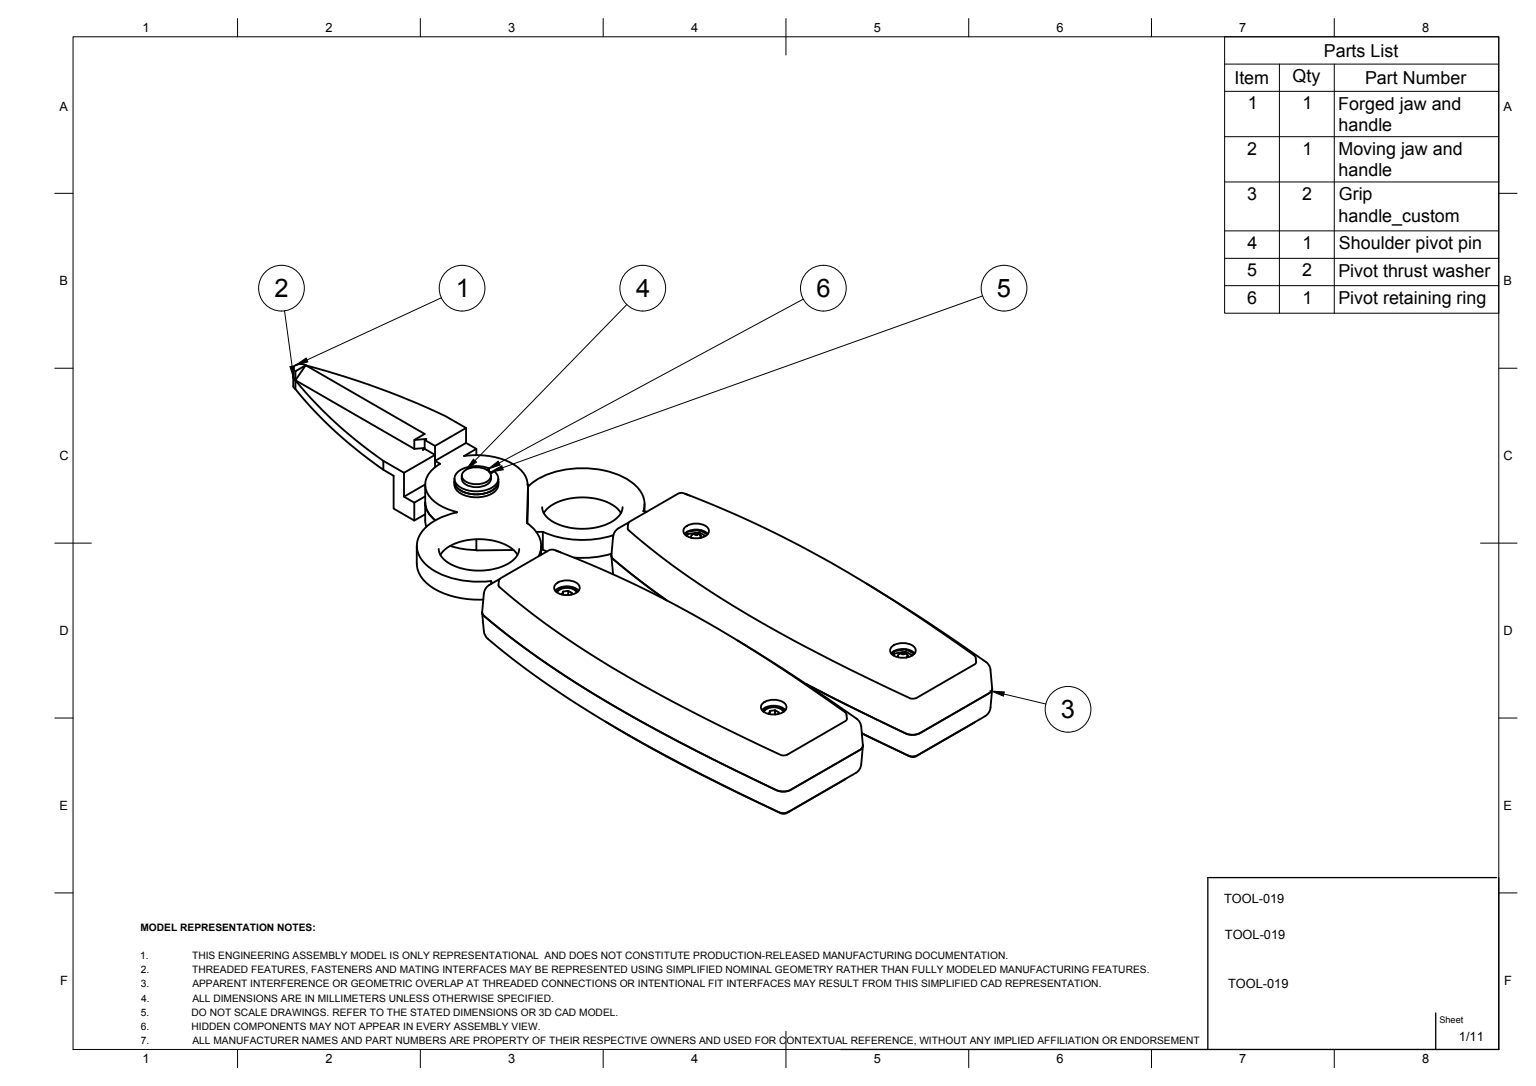
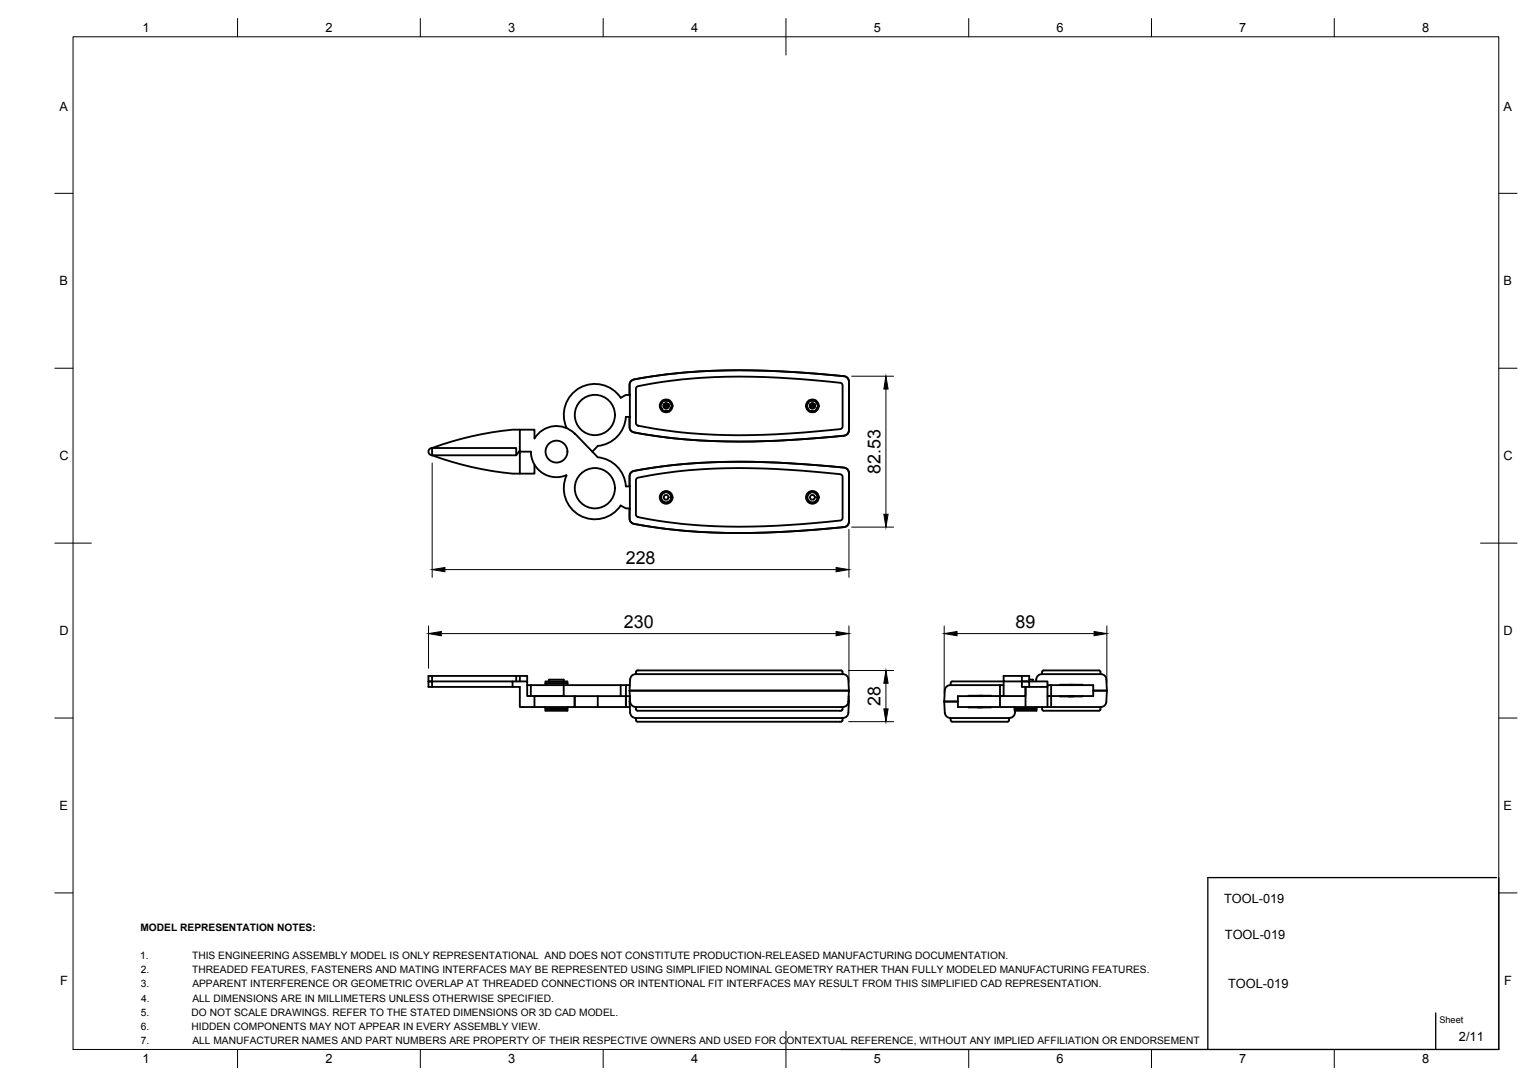
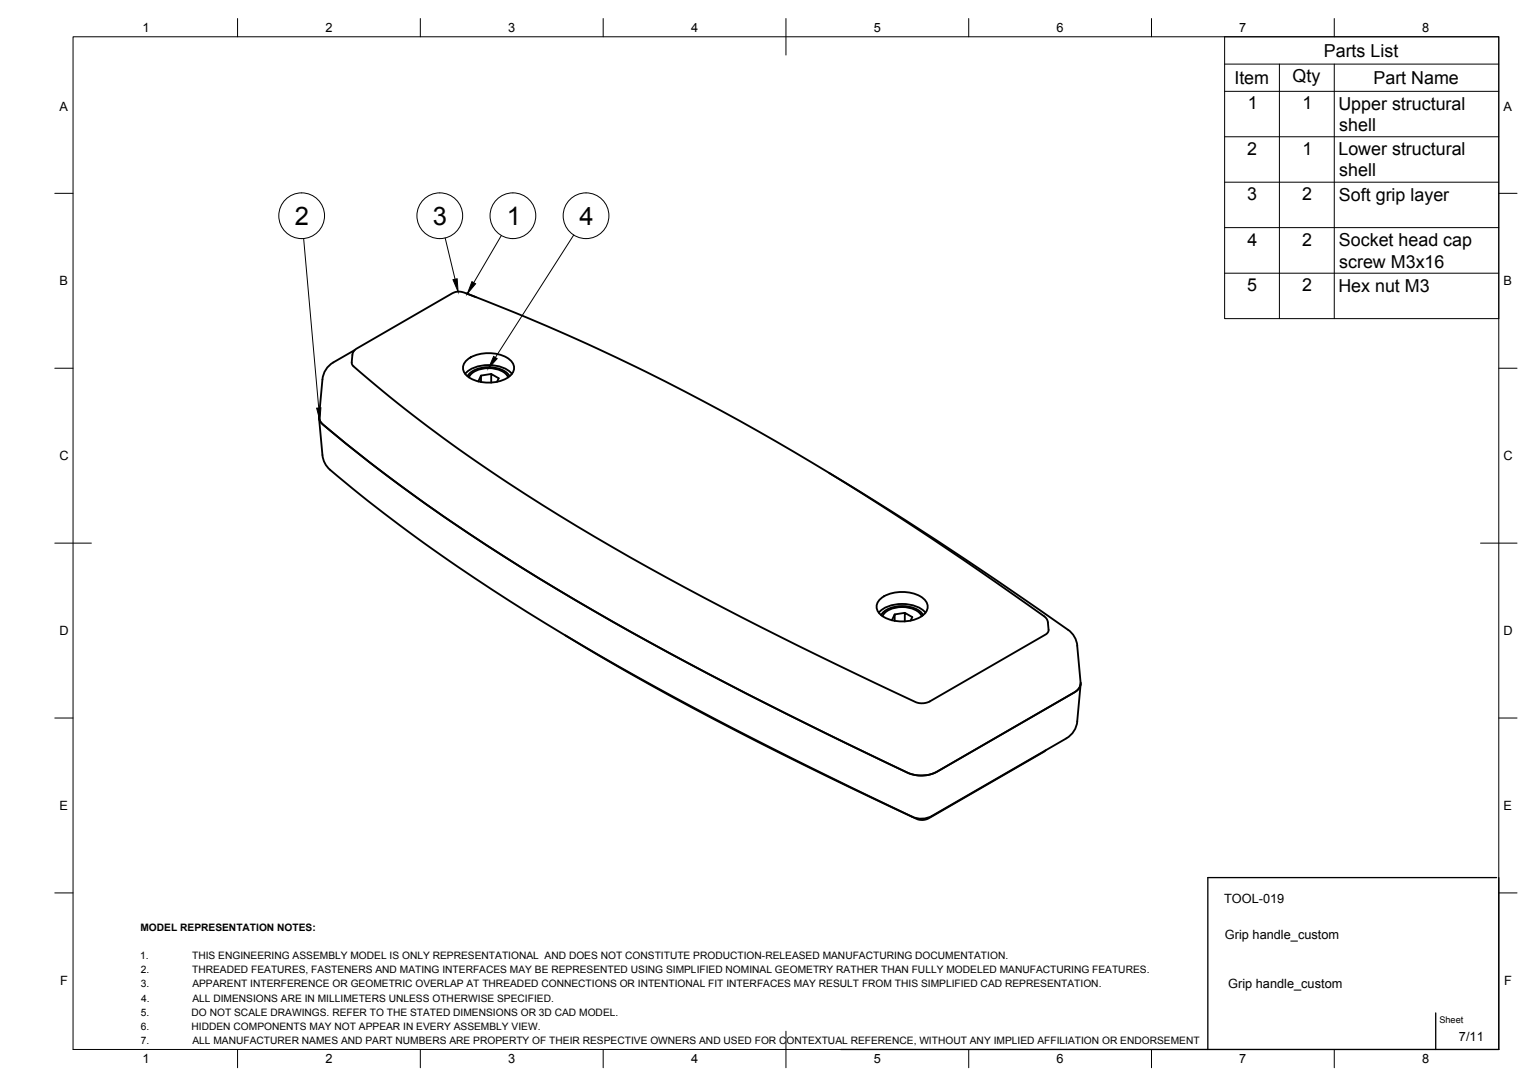
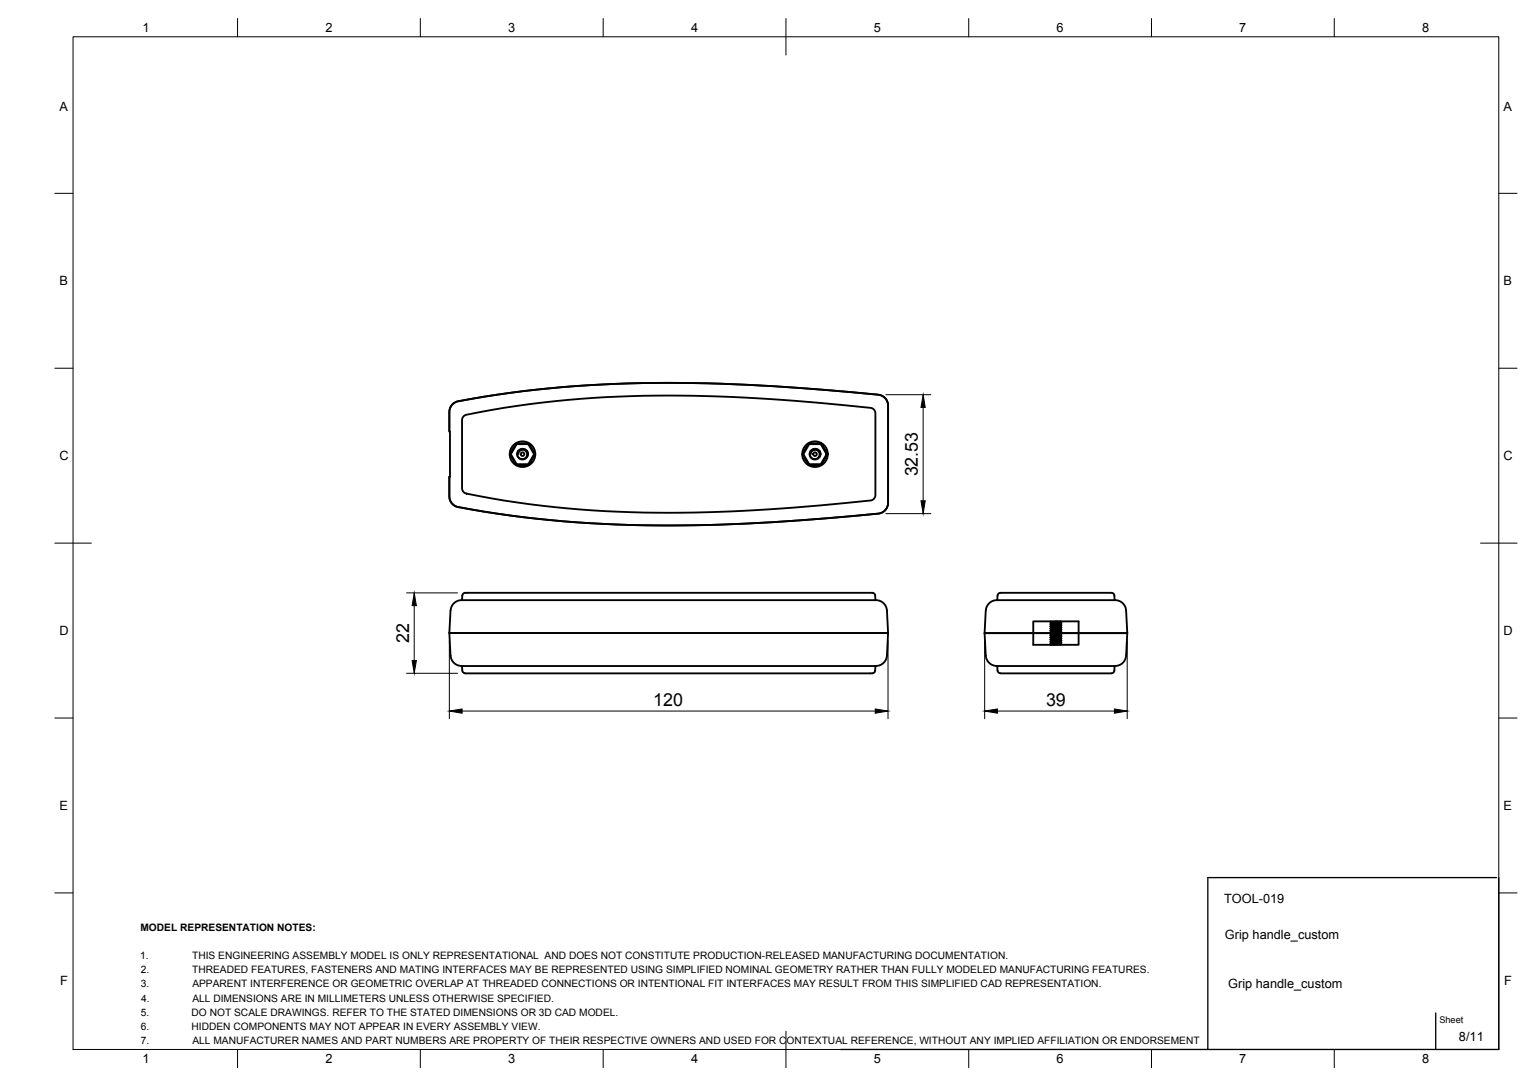
ISO-10303-21;
HEADER;
/* Generated by software containing ST-Developer
 * from STEP Tools, Inc. (www.steptools.com) 
 */

FILE_DESCRIPTION(
/* description */ (''),
/* implementation_level */ '2;1');

FILE_NAME(
/* name */ 'TOOL-019.step',
/* time_stamp */ '2026-11-10T09:14:46-08:00',
/* author */ (''),
/* organization */ (''),
/* preprocessor_version */ 'ST-DEVELOPER v20.2',
/* originating_system */ 'Autodesk Translation Framework v15.17.0.0',
/* authorisation */ '');

FILE_SCHEMA (('AUTOMOTIVE_DESIGN { 1 0 10303 214 3 1 1 }'));
ENDSEC;

DATA;
#10=MECHANICAL_DESIGN_GEOMETRIC_PRESENTATION_REPRESENTATION('',(#558,#559,
#560,#561,#562,#563,#564,#565,#566,#567),#19471);
#11=ITEM_DEFINED_TRANSFORMATION($,$,#7423,#7794);
#12=ITEM_DEFINED_TRANSFORMATION($,$,#7525,#7795);
#13=ITEM_DEFINED_TRANSFORMATION($,$,#7633,#7796);
#14=ITEM_DEFINED_TRANSFORMATION($,$,#7686,#7797);
#15=ITEM_DEFINED_TRANSFORMATION($,$,#7768,#7798);
#16=ITEM_DEFINED_TRANSFORMATION($,$,#7633,#7799);
#17=ITEM_DEFINED_TRANSFORMATION($,$,#7686,#7800);
#18=ITEM_DEFINED_TRANSFORMATION($,$,#7768,#7801);
#19=ITEM_DEFINED_TRANSFORMATION($,$,#7273,#7811);
#20=ITEM_DEFINED_TRANSFORMATION($,$,#7333,#7812);
#21=ITEM_DEFINED_TRANSFORMATION($,$,#7422,#7813);
#22=ITEM_DEFINED_TRANSFORMATION($,$,#7393,#7814);
#23=ITEM_DEFINED_TRANSFORMATION($,$,#7802,#7815);
#24=ITEM_DEFINED_TRANSFORMATION($,$,#7411,#7816);
#25=ITEM_DEFINED_TRANSFORMATION($,$,#7422,#7817);
#26=ITEM_DEFINED_TRANSFORMATION($,$,#7802,#7818);
#27=(
REPRESENTATION_RELATIONSHIP($,$,#19522,#19521)
REPRESENTATION_RELATIONSHIP_WITH_TRANSFORMATION(#11)
SHAPE_REPRESENTATION_RELATIONSHIP()
);
#28=(
REPRESENTATION_RELATIONSHIP($,$,#19523,#19521)
REPRESENTATION_RELATIONSHIP_WITH_TRANSFORMATION(#12)
SHAPE_REPRESENTATION_RELATIONSHIP()
);
#29=(
REPRESENTATION_RELATIONSHIP($,$,#19524,#19521)
REPRESENTATION_RELATIONSHIP_WITH_TRANSFORMATION(#13)
SHAPE_REPRESENTATION_RELATIONSHIP()
);
#30=(
REPRESENTATION_RELATIONSHIP($,$,#19525,#19521)
REPRESENTATION_RELATIONSHIP_WITH_TRANSFORMATION(#14)
SHAPE_REPRESENTATION_RELATIONSHIP()
);
#31=(
REPRESENTATION_RELATIONSHIP($,$,#19526,#19521)
REPRESENTATION_RELATIONSHIP_WITH_TRANSFORMATION(#15)
SHAPE_REPRESENTATION_RELATIONSHIP()
);
#32=(
REPRESENTATION_RELATIONSHIP($,$,#19524,#19521)
REPRESENTATION_RELATIONSHIP_WITH_TRANSFORMATION(#16)
SHAPE_REPRESENTATION_RELATIONSHIP()
);
#33=(
REPRESENTATION_RELATIONSHIP($,$,#19525,#19521)
REPRESENTATION_RELATIONSHIP_WITH_TRANSFORMATION(#17)
SHAPE_REPRESENTATION_RELATIONSHIP()
);
#34=(
REPRESENTATION_RELATIONSHIP($,$,#19526,#19521)
REPRESENTATION_RELATIONSHIP_WITH_TRANSFORMATION(#18)
SHAPE_REPRESENTATION_RELATIONSHIP()
);
#35=(
REPRESENTATION_RELATIONSHIP($,$,#19517,#19516)
REPRESENTATION_RELATIONSHIP_WITH_TRANSFORMATION(#19)
SHAPE_REPRESENTATION_RELATIONSHIP()
);
#36=(
REPRESENTATION_RELATIONSHIP($,$,#19518,#19516)
REPRESENTATION_RELATIONSHIP_WITH_TRANSFORMATION(#20)
SHAPE_REPRESENTATION_RELATIONSHIP()
);
#37=(
REPRESENTATION_RELATIONSHIP($,$,#19521,#19516)
REPRESENTATION_RELATIONSHIP_WITH_TRANSFORMATION(#21)
SHAPE_REPRESENTATION_RELATIONSHIP()
);
#38=(
REPRESENTATION_RELATIONSHIP($,$,#19519,#19516)
REPRESENTATION_RELATIONSHIP_WITH_TRANSFORMATION(#22)
SHAPE_REPRESENTATION_RELATIONSHIP()
);
#39=(
REPRESENTATION_RELATIONSHIP($,$,#19527,#19516)
REPRESENTATION_RELATIONSHIP_WITH_TRANSFORMATION(#23)
SHAPE_REPRESENTATION_RELATIONSHIP()
);
#40=(
REPRESENTATION_RELATIONSHIP($,$,#19520,#19516)
REPRESENTATION_RELATIONSHIP_WITH_TRANSFORMATION(#24)
SHAPE_REPRESENTATION_RELATIONSHIP()
);
#41=(
REPRESENTATION_RELATIONSHIP($,$,#19521,#19516)
REPRESENTATION_RELATIONSHIP_WITH_TRANSFORMATION(#25)
SHAPE_REPRESENTATION_RELATIONSHIP()
);
#42=(
REPRESENTATION_RELATIONSHIP($,$,#19527,#19516)
REPRESENTATION_RELATIONSHIP_WITH_TRANSFORMATION(#26)
SHAPE_REPRESENTATION_RELATIONSHIP()
);
#43=CONTEXT_DEPENDENT_SHAPE_REPRESENTATION(#27,#19499);
#44=CONTEXT_DEPENDENT_SHAPE_REPRESENTATION(#28,#19500);
#45=CONTEXT_DEPENDENT_SHAPE_REPRESENTATION(#29,#19501);
#46=CONTEXT_DEPENDENT_SHAPE_REPRESENTATION(#30,#19502);
#47=CONTEXT_DEPENDENT_SHAPE_REPRESENTATION(#31,#19503);
#48=CONTEXT_DEPENDENT_SHAPE_REPRESENTATION(#32,#19504);
#49=CONTEXT_DEPENDENT_SHAPE_REPRESENTATION(#33,#19505);
#50=CONTEXT_DEPENDENT_SHAPE_REPRESENTATION(#34,#19506);
#51=CONTEXT_DEPENDENT_SHAPE_REPRESENTATION(#35,#19508);
#52=CONTEXT_DEPENDENT_SHAPE_REPRESENTATION(#36,#19509);
#53=CONTEXT_DEPENDENT_SHAPE_REPRESENTATION(#37,#19510);
#54=CONTEXT_DEPENDENT_SHAPE_REPRESENTATION(#38,#19511);
#55=CONTEXT_DEPENDENT_SHAPE_REPRESENTATION(#39,#19512);
#56=CONTEXT_DEPENDENT_SHAPE_REPRESENTATION(#40,#19513);
#57=CONTEXT_DEPENDENT_SHAPE_REPRESENTATION(#41,#19514);
#58=CONTEXT_DEPENDENT_SHAPE_REPRESENTATION(#42,#19515);
#59=NEXT_ASSEMBLY_USAGE_OCCURRENCE('Upper structural shell:1',
'Upper structural shell:1','Upper structural shell:1',#19534,#19535,
'Upper structural shell:1');
#60=NEXT_ASSEMBLY_USAGE_OCCURRENCE('Lower structural shell:1',
'Lower structural shell:1','Lower structural shell:1',#19534,#19536,
'Lower structural shell:1');
#61=NEXT_ASSEMBLY_USAGE_OCCURRENCE('Soft grip layer:1',
'Soft grip layer:1','Soft grip layer:1',#19534,#19537,
'Soft grip layer:1');
#62=NEXT_ASSEMBLY_USAGE_OCCURRENCE('Socket head cap screw M3x16:1',
'Socket head cap screw M3x16:1','Socket head cap screw M3x16:1',#19534,
#19538,'Socket head cap screw M3x16:1');
#63=NEXT_ASSEMBLY_USAGE_OCCURRENCE('Hex nut M3:1','Hex nut M3:1',
'Hex nut M3:1',#19534,#19539,'Hex nut M3:1');
#64=NEXT_ASSEMBLY_USAGE_OCCURRENCE('Soft grip layer:2',
'Soft grip layer:2','Soft grip layer:2',#19534,#19537,
'Soft grip layer:2');
#65=NEXT_ASSEMBLY_USAGE_OCCURRENCE('Socket head cap screw M3x16:2',
'Socket head cap screw M3x16:2','Socket head cap screw M3x16:2',#19534,
#19538,'Socket head cap screw M3x16:2');
#66=NEXT_ASSEMBLY_USAGE_OCCURRENCE('Hex nut M3:2','Hex nut M3:2',
'Hex nut M3:2',#19534,#19539,'Hex nut M3:2');
#67=NEXT_ASSEMBLY_USAGE_OCCURRENCE('Forged jaw and handle:1',
'Forged jaw and handle:1','Forged jaw and handle:1',#19529,#19530,
'Forged jaw and handle:1');
#68=NEXT_ASSEMBLY_USAGE_OCCURRENCE('Moving jaw and handle:1',
'Moving jaw and handle:1','Moving jaw and handle:1',#19529,#19531,
'Moving jaw and handle:1');
#69=NEXT_ASSEMBLY_USAGE_OCCURRENCE('Grip handle_custom:1',
'Grip handle_custom:1','Grip handle_custom:1',#19529,#19534,
'Grip handle_custom:1');
#70=NEXT_ASSEMBLY_USAGE_OCCURRENCE('Shoulder pivot pin:1',
'Shoulder pivot pin:1','Shoulder pivot pin:1',#19529,#19532,
'Shoulder pivot pin:1');
#71=NEXT_ASSEMBLY_USAGE_OCCURRENCE('Pivot thrust washer:1',
'Pivot thrust washer:1','Pivot thrust washer:1',#19529,#19540,
'Pivot thrust washer:1');
#72=NEXT_ASSEMBLY_USAGE_OCCURRENCE('Pivot retaining ring:1',
'Pivot retaining ring:1','Pivot retaining ring:1',#19529,#19533,
'Pivot retaining ring:1');
#73=NEXT_ASSEMBLY_USAGE_OCCURRENCE('Grip handle_custom:2',
'Grip handle_custom:2','Grip handle_custom:2',#19529,#19534,
'Grip handle_custom:2');
#74=NEXT_ASSEMBLY_USAGE_OCCURRENCE('Pivot thrust washer:2',
'Pivot thrust washer:2','Pivot thrust washer:2',#19529,#19540,
'Pivot thrust washer:2');
#75=CONICAL_SURFACE('',#7749,0.1,0.785398163397448);
#76=SPHERICAL_SURFACE('',#7488,0.0999999999999999);
#77=SPHERICAL_SURFACE('',#7491,0.100000000000002);
#78=SPHERICAL_SURFACE('',#7495,0.0999999999999991);
#79=SPHERICAL_SURFACE('',#7499,0.1);
#80=SPHERICAL_SURFACE('',#7504,0.3);
#81=SPHERICAL_SURFACE('',#7508,0.300000000000002);
#82=SPHERICAL_SURFACE('',#7512,0.299999999999999);
#83=SPHERICAL_SURFACE('',#7517,0.3);
#84=SPHERICAL_SURFACE('',#7596,0.0999999999999999);
#85=SPHERICAL_SURFACE('',#7599,0.100000000000002);
#86=SPHERICAL_SURFACE('',#7603,0.0999999999999991);
#87=SPHERICAL_SURFACE('',#7607,0.1);
#88=SPHERICAL_SURFACE('',#7612,0.3);
#89=SPHERICAL_SURFACE('',#7616,0.300000000000002);
#90=SPHERICAL_SURFACE('',#7620,0.299999999999999);
#91=SPHERICAL_SURFACE('',#7625,0.3);
#92=B_SPLINE_SURFACE_WITH_KNOTS('',3,3,((#10686,#10687,#10688,#10689),(#10690,
#10691,#10692,#10693),(#10694,#10695,#10696,#10697),(#10698,#10699,#10700,
#10701)),.UNSPECIFIED.,.F.,.F.,.F.,(4,4),(4,4),(0.0627625298587661,0.3242096015809),
(0.0118073085896899,0.685451490706028),.UNSPECIFIED.);
#93=B_SPLINE_SURFACE_WITH_KNOTS('',3,3,((#10706,#10707,#10708,#10709),(#10710,
#10711,#10712,#10713),(#10714,#10715,#10716,#10717),(#10718,#10719,#10720,
#10721)),.UNSPECIFIED.,.F.,.F.,.F.,(4,4),(4,4),(0.0225360950145449,0.0483865590996774),
(0.0125659096559557,0.685650832343257),.UNSPECIFIED.);
#94=B_SPLINE_SURFACE_WITH_KNOTS('',3,3,((#10731,#10732,#10733,#10734),(#10735,
#10736,#10737,#10738),(#10739,#10740,#10741,#10742),(#10743,#10744,#10745,
#10746),(#10747,#10748,#10749,#10750)),.UNSPECIFIED.,.F.,.F.,.F.,(4,1,4),
(4,4),(0.,0.571428571428571,1.),(0.74118252158834,3.85438678954986),
 .UNSPECIFIED.);
#95=B_SPLINE_SURFACE_WITH_KNOTS('',3,3,((#10755,#10756,#10757,#10758),(#10759,
#10760,#10761,#10762),(#10763,#10764,#10765,#10766),(#10767,#10768,#10769,
#10770),(#10771,#10772,#10773,#10774)),.UNSPECIFIED.,.F.,.F.,.F.,(4,1,4),
(4,4),(0.,0.571428571428571,1.),(0.270878787657975,0.54981857912664),
 .UNSPECIFIED.);
#96=B_SPLINE_SURFACE_WITH_KNOTS('',3,3,((#10793,#10794,#10795,#10796),(#10797,
#10798,#10799,#10800),(#10801,#10802,#10803,#10804),(#10805,#10806,#10807,
#10808),(#10809,#10810,#10811,#10812)),.UNSPECIFIED.,.F.,.F.,.F.,(4,1,4),
(4,4),(0.,0.571428571428571,1.),(8.03948512627517,11.1526893942367),
 .UNSPECIFIED.);
#97=B_SPLINE_SURFACE_WITH_KNOTS('',3,3,((#10817,#10818,#10819,#10820),(#10821,
#10822,#10823,#10824),(#10825,#10826,#10827,#10828),(#10829,#10830,#10831,
#10832)),.UNSPECIFIED.,.F.,.F.,.F.,(4,4),(4,4),(0.675790398419059,0.937237470141233),
(0.0118073085603101,0.685451490706029),.UNSPECIFIED.);
#98=B_SPLINE_SURFACE_WITH_KNOTS('',3,3,((#10833,#10834,#10835,#10836),(#10837,
#10838,#10839,#10840),(#10841,#10842,#10843,#10844),(#10845,#10846,#10847,
#10848)),.UNSPECIFIED.,.F.,.F.,.F.,(4,4),(4,4),(0.951613440900322,0.977463904985455),
(0.0125659096559558,0.685650832343257),.UNSPECIFIED.);
#99=B_SPLINE_SURFACE_WITH_KNOTS('',3,3,((#10932,#10933,#10934,#10935),(#10936,
#10937,#10938,#10939),(#10940,#10941,#10942,#10943),(#10944,#10945,#10946,
#10947)),.UNSPECIFIED.,.F.,.F.,.F.,(4,4),(4,4),(0.340089900275858,0.660082688299826),
(0.0116294244283504,0.684384408933581),.UNSPECIFIED.);
#100=B_SPLINE_SURFACE_WITH_KNOTS('',3,3,((#10952,#10953,#10954,#10955),
(#10956,#10957,#10958,#10959),(#10960,#10961,#10962,#10963),(#10964,#10965,
#10966,#10967),(#10968,#10969,#10970,#10971)),.UNSPECIFIED.,.F.,.F.,.F.,
(4,1,4),(4,4),(0.,0.571428571428571,1.),(4.04989375377528,7.85140214144331),
 .UNSPECIFIED.);
#101=B_SPLINE_SURFACE_WITH_KNOTS('',3,3,((#10981,#10982,#10983,#10984),
(#10985,#10986,#10987,#10988),(#10989,#10990,#10991,#10992),(#10993,#10994,
#10995,#10996),(#10997,#10998,#10999,#11000)),.UNSPECIFIED.,.F.,.F.,.F.,
(4,1,4),(4,4),(0.,0.571428571428571,1.),(4.0424697743818,7.84397816204974),
 .UNSPECIFIED.);
#102=B_SPLINE_SURFACE_WITH_KNOTS('',3,3,((#11005,#11006,#11007,#11008),
(#11009,#11010,#11011,#11012),(#11013,#11014,#11015,#11016),(#11017,#11018,
#11019,#11020)),.UNSPECIFIED.,.F.,.F.,.F.,(4,4),(4,4),(0.339917311700174,
0.659910099724142),(0.0116294573698948,0.684384408933581),.UNSPECIFIED.);
#103=B_SPLINE_SURFACE_WITH_KNOTS('',3,3,((#11095,#11096,#11097,#11098),
(#11099,#11100,#11101,#11102),(#11103,#11104,#11105,#11106),(#11107,#11108,
#11109,#11110)),.UNSPECIFIED.,.F.,.F.,.F.,(4,4),(4,4),(0.675996615945502,
0.913173856075534),(0.0118505108223707,0.686152089762332),.UNSPECIFIED.);
#104=B_SPLINE_SURFACE_WITH_KNOTS('',3,3,((#11115,#11116,#11117,#11118),
(#11119,#11120,#11121,#11122),(#11123,#11124,#11125,#11126),(#11127,#11128,
#11129,#11130),(#11131,#11132,#11133,#11134)),.UNSPECIFIED.,.F.,.F.,.F.,
(4,1,4),(4,4),(0.,0.571428571428571,1.),(8.0457708503995,10.8690635835914),
 .UNSPECIFIED.);
#105=B_SPLINE_SURFACE_WITH_KNOTS('',3,3,((#11144,#11145,#11146,#11147),
(#11148,#11149,#11150,#11151),(#11152,#11153,#11154,#11155),(#11156,#11157,
#11158,#11159),(#11160,#11161,#11162,#11163)),.UNSPECIFIED.,.F.,.F.,.F.,
(4,1,4),(4,4),(0.,0.571428571428571,1.),(1.02480833223363,3.8481010654256),
 .UNSPECIFIED.);
#106=B_SPLINE_SURFACE_WITH_KNOTS('',3,3,((#11168,#11169,#11170,#11171),
(#11172,#11173,#11174,#11175),(#11176,#11177,#11178,#11179),(#11180,#11181,
#11182,#11183)),.UNSPECIFIED.,.F.,.F.,.F.,(4,4),(4,4),(0.0868261439244655,
0.324003384054498),(0.0118505108223707,0.686152089762332),.UNSPECIFIED.);
#107=B_SPLINE_SURFACE_WITH_KNOTS('',3,3,((#11258,#11259,#11260,#11261),
(#11262,#11263,#11264,#11265),(#11266,#11267,#11268,#11269),(#11270,#11271,
#11272,#11273)),.UNSPECIFIED.,.F.,.F.,.F.,(4,4),(4,4),(0.927751606342899,
0.979699913047832),(0.0130895688562318,0.686930956013783),.UNSPECIFIED.);
#108=B_SPLINE_SURFACE_WITH_KNOTS('',3,3,((#11283,#11284,#11285,#11286),
(#11287,#11288,#11289,#11290),(#11291,#11292,#11293,#11294),(#11295,#11296,
#11297,#11298),(#11299,#11300,#11301,#11302)),.UNSPECIFIED.,.F.,.F.,.F.,
(4,1,4),(4,4),(0.,0.571428571428571,1.),(11.0550486447215,11.6488871259622),
 .UNSPECIFIED.);
#109=B_SPLINE_SURFACE_WITH_KNOTS('',3,3,((#11316,#11317,#11318,#11319),
(#11320,#11321,#11322,#11323),(#11324,#11325,#11326,#11327),(#11328,#11329,
#11330,#11331)),.UNSPECIFIED.,.F.,.F.,.F.,(4,4),(4,4),(0.0203000869521683,
0.0722483936571013),(0.0130895688562318,0.686930956013783),
 .UNSPECIFIED.);
#110=B_SPLINE_SURFACE_WITH_KNOTS('',3,3,((#11341,#11342,#11343,#11344),
(#11345,#11346,#11347,#11348),(#11349,#11350,#11351,#11352),(#11353,#11354,
#11355,#11356),(#11357,#11358,#11359,#11360)),.UNSPECIFIED.,.F.,.F.,.F.,
(4,1,4),(4,4),(0.,0.571428571428571,1.),(0.244984789862841,0.838823271103535),
 .UNSPECIFIED.);
#111=B_SPLINE_SURFACE_WITH_KNOTS('',3,3,((#11374,#11375,#11376,#11377),
(#11378,#11379,#11380,#11381),(#11382,#11383,#11384,#11385),(#11386,#11387,
#11388,#11389),(#11390,#11391,#11392,#11393)),.UNSPECIFIED.,.F.,.F.,.F.,
(4,1,4),(4,4),(0.,0.5,1.),(0.0108921325678979,0.619909717328002),
 .UNSPECIFIED.);
#112=B_SPLINE_SURFACE_WITH_KNOTS('',3,3,((#11400,#11401,#11402,#11403),
(#11404,#11405,#11406,#11407),(#11408,#11409,#11410,#11411),(#11412,#11413,
#11414,#11415),(#11416,#11417,#11418,#11419)),.UNSPECIFIED.,.F.,.F.,.F.,
(4,1,4),(4,4),(0.,0.571428571428571,1.),(0.00967450486392679,0.618764321025346),
 .UNSPECIFIED.);
#113=B_SPLINE_SURFACE_WITH_KNOTS('',3,3,((#11424,#11425,#11426,#11427),
(#11428,#11429,#11430,#11431),(#11432,#11433,#11434,#11435),(#11436,#11437,
#11438,#11439),(#11440,#11441,#11442,#11443)),.UNSPECIFIED.,.F.,.F.,.F.,
(4,1,4),(4,4),(0.,0.571428571428571,1.),(0.0097274579809394,0.618764321025346),
 .UNSPECIFIED.);
#114=B_SPLINE_SURFACE_WITH_KNOTS('',3,3,((#11448,#11449,#11450,#11451),
(#11452,#11453,#11454,#11455),(#11456,#11457,#11458,#11459),(#11460,#11461,
#11462,#11463),(#11464,#11465,#11466,#11467)),.UNSPECIFIED.,.F.,.F.,.F.,
(4,1,4),(4,4),(0.,0.571428571428571,1.),(11.3440533366984,11.6229931281671),
 .UNSPECIFIED.);
#115=B_SPLINE_SURFACE_WITH_KNOTS('',3,3,((#11468,#11469,#11470,#11471),
(#11472,#11473,#11474,#11475),(#11476,#11477,#11478,#11479),(#11480,#11481,
#11482,#11483),(#11484,#11485,#11486,#11487)),.UNSPECIFIED.,.F.,.F.,.F.,
(4,1,4),(4,4),(0.,0.5,1.),(0.0108402259132964,0.619909717328002),
 .UNSPECIFIED.);
#116=B_SPLINE_SURFACE_WITH_KNOTS('',3,3,((#11513,#11514,#11515,#11516),
(#11517,#11518,#11519,#11520),(#11521,#11522,#11523,#11524),(#11525,#11526,
#11527,#11528),(#11529,#11530,#11531,#11532)),.UNSPECIFIED.,.F.,.F.,.F.,
(4,1,4),(4,4),(0.,0.571428571428571,1.),(-0.00387706229521417,0.619909717328002),
 .UNSPECIFIED.);
#117=B_SPLINE_SURFACE_WITH_KNOTS('',3,3,((#11551,#11552,#11553,#11554,#11555,
#11556),(#11557,#11558,#11559,#11560,#11561,#11562),(#11563,#11564,#11565,
#11566,#11567,#11568),(#11569,#11570,#11571,#11572,#11573,#11574),(#11575,
#11576,#11577,#11578,#11579,#11580)),.UNSPECIFIED.,.F.,.F.,.F.,(4,1,4),
(4,1,1,4),(0.,0.571428571428571,1.),(0.270878787657975,5.14716807550265,
8.39802760073243,11.6488871259622),.UNSPECIFIED.);
#118=B_SPLINE_SURFACE_WITH_KNOTS('',3,3,((#11593,#11594,#11595,#11596),
(#11597,#11598,#11599,#11600),(#11601,#11602,#11603,#11604),(#11605,#11606,
#11607,#11608),(#11609,#11610,#11611,#11612)),.UNSPECIFIED.,.F.,.F.,.F.,
(4,1,4),(4,4),(0.,0.571428571428571,1.),(-0.00522825793187074,0.618764321025346),
 .UNSPECIFIED.);
#119=B_SPLINE_SURFACE_WITH_KNOTS('',3,3,((#11621,#11622,#11623,#11624),
(#11625,#11626,#11627,#11628),(#11629,#11630,#11631,#11632),(#11633,#11634,
#11635,#11636),(#11637,#11638,#11639,#11640)),.UNSPECIFIED.,.F.,.F.,.F.,
(4,1,4),(4,4),(0.,0.571428571428571,1.),(-0.00506942997988007,0.618764321025346),
 .UNSPECIFIED.);
#120=B_SPLINE_SURFACE_WITH_KNOTS('',3,3,((#11649,#11650,#11651,#11652,#11653),
(#11654,#11655,#11656,#11657,#11658),(#11659,#11660,#11661,#11662,#11663),
(#11664,#11665,#11666,#11667,#11668),(#11669,#11670,#11671,#11672,#11673)),
 .UNSPECIFIED.,.F.,.F.,.F.,(4,1,4),(4,1,4),(0.,0.571428571428571,1.),(0.244984789862841,
5.12127407770751,11.6229931281671),.UNSPECIFIED.);
#121=B_SPLINE_SURFACE_WITH_KNOTS('',3,3,((#11684,#11685,#11686,#11687),
(#11688,#11689,#11690,#11691),(#11692,#11693,#11694,#11695),(#11696,#11697,
#11698,#11699),(#11700,#11701,#11702,#11703)),.UNSPECIFIED.,.F.,.F.,.F.,
(4,1,4),(4,4),(0.,0.571428571428571,1.),(-0.00403278922781227,0.619909717328002),
 .UNSPECIFIED.);
#122=B_SPLINE_SURFACE_WITH_KNOTS('',3,3,((#11712,#11713,#11714,#11715),
(#11716,#11717,#11718,#11719),(#11720,#11721,#11722,#11723),(#11724,#11725,
#11726,#11727)),.UNSPECIFIED.,.F.,.F.,.F.,(4,4),(4,4),(0.0225340877622934,
0.979701609653785),(0.,0.686930956013783),.UNSPECIFIED.);
#123=B_SPLINE_SURFACE_WITH_KNOTS('',3,3,((#11730,#11731,#11732,#11733),
(#11734,#11735,#11736,#11737),(#11738,#11739,#11740,#11741),(#11742,#11743,
#11744,#11745)),.UNSPECIFIED.,.F.,.F.,.F.,(4,4),(4,4),(0.0202983903462145,
0.977465912237707),(0.,0.686930956013783),.UNSPECIFIED.);
#124=B_SPLINE_SURFACE_WITH_KNOTS('',3,3,((#12681,#12682,#12683,#12684),
(#12685,#12686,#12687,#12688),(#12689,#12690,#12691,#12692),(#12693,#12694,
#12695,#12696)),.UNSPECIFIED.,.F.,.F.,.F.,(4,4),(4,4),(0.0627625298587661,
0.3242096015809),(0.0118073085896899,0.685451490706028),.UNSPECIFIED.);
#125=B_SPLINE_SURFACE_WITH_KNOTS('',3,3,((#12701,#12702,#12703,#12704),
(#12705,#12706,#12707,#12708),(#12709,#12710,#12711,#12712),(#12713,#12714,
#12715,#12716)),.UNSPECIFIED.,.F.,.F.,.F.,(4,4),(4,4),(0.0225360950145449,
0.0483865590996774),(0.0125659096559557,0.685650832343257),
 .UNSPECIFIED.);
#126=B_SPLINE_SURFACE_WITH_KNOTS('',3,3,((#12726,#12727,#12728,#12729),
(#12730,#12731,#12732,#12733),(#12734,#12735,#12736,#12737),(#12738,#12739,
#12740,#12741),(#12742,#12743,#12744,#12745)),.UNSPECIFIED.,.F.,.F.,.F.,
(4,1,4),(4,4),(0.,0.571428571428571,1.),(0.74118252158834,3.85438678954986),
 .UNSPECIFIED.);
#127=B_SPLINE_SURFACE_WITH_KNOTS('',3,3,((#12750,#12751,#12752,#12753),
(#12754,#12755,#12756,#12757),(#12758,#12759,#12760,#12761),(#12762,#12763,
#12764,#12765),(#12766,#12767,#12768,#12769)),.UNSPECIFIED.,.F.,.F.,.F.,
(4,1,4),(4,4),(0.,0.571428571428571,1.),(0.270878787657975,0.54981857912664),
 .UNSPECIFIED.);
#128=B_SPLINE_SURFACE_WITH_KNOTS('',3,3,((#12788,#12789,#12790,#12791),
(#12792,#12793,#12794,#12795),(#12796,#12797,#12798,#12799),(#12800,#12801,
#12802,#12803),(#12804,#12805,#12806,#12807)),.UNSPECIFIED.,.F.,.F.,.F.,
(4,1,4),(4,4),(0.,0.571428571428571,1.),(8.03948512627517,11.1526893942367),
 .UNSPECIFIED.);
#129=B_SPLINE_SURFACE_WITH_KNOTS('',3,3,((#12812,#12813,#12814,#12815),
(#12816,#12817,#12818,#12819),(#12820,#12821,#12822,#12823),(#12824,#12825,
#12826,#12827)),.UNSPECIFIED.,.F.,.F.,.F.,(4,4),(4,4),(0.675790398419059,
0.937237470141233),(0.0118073085603101,0.685451490706029),.UNSPECIFIED.);
#130=B_SPLINE_SURFACE_WITH_KNOTS('',3,3,((#12828,#12829,#12830,#12831),
(#12832,#12833,#12834,#12835),(#12836,#12837,#12838,#12839),(#12840,#12841,
#12842,#12843)),.UNSPECIFIED.,.F.,.F.,.F.,(4,4),(4,4),(0.951613440900322,
0.977463904985455),(0.0125659096559558,0.685650832343257),.UNSPECIFIED.);
#131=B_SPLINE_SURFACE_WITH_KNOTS('',3,3,((#12927,#12928,#12929,#12930),
(#12931,#12932,#12933,#12934),(#12935,#12936,#12937,#12938),(#12939,#12940,
#12941,#12942)),.UNSPECIFIED.,.F.,.F.,.F.,(4,4),(4,4),(0.340089900275858,
0.660082688299826),(0.0116294244283504,0.684384408933581),.UNSPECIFIED.);
#132=B_SPLINE_SURFACE_WITH_KNOTS('',3,3,((#12947,#12948,#12949,#12950),
(#12951,#12952,#12953,#12954),(#12955,#12956,#12957,#12958),(#12959,#12960,
#12961,#12962),(#12963,#12964,#12965,#12966)),.UNSPECIFIED.,.F.,.F.,.F.,
(4,1,4),(4,4),(0.,0.571428571428571,1.),(4.04989375377528,7.85140214144331),
 .UNSPECIFIED.);
#133=B_SPLINE_SURFACE_WITH_KNOTS('',3,3,((#12976,#12977,#12978,#12979),
(#12980,#12981,#12982,#12983),(#12984,#12985,#12986,#12987),(#12988,#12989,
#12990,#12991),(#12992,#12993,#12994,#12995)),.UNSPECIFIED.,.F.,.F.,.F.,
(4,1,4),(4,4),(0.,0.571428571428571,1.),(4.0424697743818,7.84397816204974),
 .UNSPECIFIED.);
#134=B_SPLINE_SURFACE_WITH_KNOTS('',3,3,((#13000,#13001,#13002,#13003),
(#13004,#13005,#13006,#13007),(#13008,#13009,#13010,#13011),(#13012,#13013,
#13014,#13015)),.UNSPECIFIED.,.F.,.F.,.F.,(4,4),(4,4),(0.339917311700174,
0.659910099724142),(0.0116294573698948,0.684384408933581),.UNSPECIFIED.);
#135=B_SPLINE_SURFACE_WITH_KNOTS('',3,3,((#13090,#13091,#13092,#13093),
(#13094,#13095,#13096,#13097),(#13098,#13099,#13100,#13101),(#13102,#13103,
#13104,#13105)),.UNSPECIFIED.,.F.,.F.,.F.,(4,4),(4,4),(0.675996615945502,
0.913173856075534),(0.0118505108223707,0.686152089762332),.UNSPECIFIED.);
#136=B_SPLINE_SURFACE_WITH_KNOTS('',3,3,((#13110,#13111,#13112,#13113),
(#13114,#13115,#13116,#13117),(#13118,#13119,#13120,#13121),(#13122,#13123,
#13124,#13125),(#13126,#13127,#13128,#13129)),.UNSPECIFIED.,.F.,.F.,.F.,
(4,1,4),(4,4),(0.,0.571428571428571,1.),(8.0457708503995,10.8690635835914),
 .UNSPECIFIED.);
#137=B_SPLINE_SURFACE_WITH_KNOTS('',3,3,((#13139,#13140,#13141,#13142),
(#13143,#13144,#13145,#13146),(#13147,#13148,#13149,#13150),(#13151,#13152,
#13153,#13154),(#13155,#13156,#13157,#13158)),.UNSPECIFIED.,.F.,.F.,.F.,
(4,1,4),(4,4),(0.,0.571428571428571,1.),(1.02480833223363,3.8481010654256),
 .UNSPECIFIED.);
#138=B_SPLINE_SURFACE_WITH_KNOTS('',3,3,((#13163,#13164,#13165,#13166),
(#13167,#13168,#13169,#13170),(#13171,#13172,#13173,#13174),(#13175,#13176,
#13177,#13178)),.UNSPECIFIED.,.F.,.F.,.F.,(4,4),(4,4),(0.0868261439244655,
0.324003384054498),(0.0118505108223707,0.686152089762332),.UNSPECIFIED.);
#139=B_SPLINE_SURFACE_WITH_KNOTS('',3,3,((#13253,#13254,#13255,#13256),
(#13257,#13258,#13259,#13260),(#13261,#13262,#13263,#13264),(#13265,#13266,
#13267,#13268)),.UNSPECIFIED.,.F.,.F.,.F.,(4,4),(4,4),(0.927751606342899,
0.979699913047832),(0.0130895688562318,0.686930956013783),.UNSPECIFIED.);
#140=B_SPLINE_SURFACE_WITH_KNOTS('',3,3,((#13278,#13279,#13280,#13281),
(#13282,#13283,#13284,#13285),(#13286,#13287,#13288,#13289),(#13290,#13291,
#13292,#13293),(#13294,#13295,#13296,#13297)),.UNSPECIFIED.,.F.,.F.,.F.,
(4,1,4),(4,4),(0.,0.571428571428571,1.),(11.0550486447215,11.6488871259622),
 .UNSPECIFIED.);
#141=B_SPLINE_SURFACE_WITH_KNOTS('',3,3,((#13311,#13312,#13313,#13314),
(#13315,#13316,#13317,#13318),(#13319,#13320,#13321,#13322),(#13323,#13324,
#13325,#13326)),.UNSPECIFIED.,.F.,.F.,.F.,(4,4),(4,4),(0.0203000869521683,
0.0722483936571013),(0.0130895688562318,0.686930956013783),
 .UNSPECIFIED.);
#142=B_SPLINE_SURFACE_WITH_KNOTS('',3,3,((#13336,#13337,#13338,#13339),
(#13340,#13341,#13342,#13343),(#13344,#13345,#13346,#13347),(#13348,#13349,
#13350,#13351),(#13352,#13353,#13354,#13355)),.UNSPECIFIED.,.F.,.F.,.F.,
(4,1,4),(4,4),(0.,0.571428571428571,1.),(0.244984789862841,0.838823271103535),
 .UNSPECIFIED.);
#143=B_SPLINE_SURFACE_WITH_KNOTS('',3,3,((#13369,#13370,#13371,#13372),
(#13373,#13374,#13375,#13376),(#13377,#13378,#13379,#13380),(#13381,#13382,
#13383,#13384),(#13385,#13386,#13387,#13388)),.UNSPECIFIED.,.F.,.F.,.F.,
(4,1,4),(4,4),(0.,0.5,1.),(0.0108921325678979,0.619909717328002),
 .UNSPECIFIED.);
#144=B_SPLINE_SURFACE_WITH_KNOTS('',3,3,((#13395,#13396,#13397,#13398),
(#13399,#13400,#13401,#13402),(#13403,#13404,#13405,#13406),(#13407,#13408,
#13409,#13410),(#13411,#13412,#13413,#13414)),.UNSPECIFIED.,.F.,.F.,.F.,
(4,1,4),(4,4),(0.,0.571428571428571,1.),(0.00967450486392679,0.618764321025346),
 .UNSPECIFIED.);
#145=B_SPLINE_SURFACE_WITH_KNOTS('',3,3,((#13419,#13420,#13421,#13422),
(#13423,#13424,#13425,#13426),(#13427,#13428,#13429,#13430),(#13431,#13432,
#13433,#13434),(#13435,#13436,#13437,#13438)),.UNSPECIFIED.,.F.,.F.,.F.,
(4,1,4),(4,4),(0.,0.571428571428571,1.),(0.0097274579809394,0.618764321025346),
 .UNSPECIFIED.);
#146=B_SPLINE_SURFACE_WITH_KNOTS('',3,3,((#13443,#13444,#13445,#13446),
(#13447,#13448,#13449,#13450),(#13451,#13452,#13453,#13454),(#13455,#13456,
#13457,#13458),(#13459,#13460,#13461,#13462)),.UNSPECIFIED.,.F.,.F.,.F.,
(4,1,4),(4,4),(0.,0.571428571428571,1.),(11.3440533366984,11.6229931281671),
 .UNSPECIFIED.);
#147=B_SPLINE_SURFACE_WITH_KNOTS('',3,3,((#13463,#13464,#13465,#13466),
(#13467,#13468,#13469,#13470),(#13471,#13472,#13473,#13474),(#13475,#13476,
#13477,#13478),(#13479,#13480,#13481,#13482)),.UNSPECIFIED.,.F.,.F.,.F.,
(4,1,4),(4,4),(0.,0.5,1.),(0.0108402259132964,0.619909717328002),
 .UNSPECIFIED.);
#148=B_SPLINE_SURFACE_WITH_KNOTS('',3,3,((#13508,#13509,#13510,#13511),
(#13512,#13513,#13514,#13515),(#13516,#13517,#13518,#13519),(#13520,#13521,
#13522,#13523),(#13524,#13525,#13526,#13527)),.UNSPECIFIED.,.F.,.F.,.F.,
(4,1,4),(4,4),(0.,0.571428571428571,1.),(-0.00387706229521417,0.619909717328002),
 .UNSPECIFIED.);
#149=B_SPLINE_SURFACE_WITH_KNOTS('',3,3,((#13546,#13547,#13548,#13549,#13550,
#13551),(#13552,#13553,#13554,#13555,#13556,#13557),(#13558,#13559,#13560,
#13561,#13562,#13563),(#13564,#13565,#13566,#13567,#13568,#13569),(#13570,
#13571,#13572,#13573,#13574,#13575)),.UNSPECIFIED.,.F.,.F.,.F.,(4,1,4),
(4,1,1,4),(0.,0.571428571428571,1.),(0.270878787657975,5.14716807550265,
8.39802760073243,11.6488871259622),.UNSPECIFIED.);
#150=B_SPLINE_SURFACE_WITH_KNOTS('',3,3,((#13588,#13589,#13590,#13591),
(#13592,#13593,#13594,#13595),(#13596,#13597,#13598,#13599),(#13600,#13601,
#13602,#13603),(#13604,#13605,#13606,#13607)),.UNSPECIFIED.,.F.,.F.,.F.,
(4,1,4),(4,4),(0.,0.571428571428571,1.),(-0.00522825793187074,0.618764321025346),
 .UNSPECIFIED.);
#151=B_SPLINE_SURFACE_WITH_KNOTS('',3,3,((#13616,#13617,#13618,#13619),
(#13620,#13621,#13622,#13623),(#13624,#13625,#13626,#13627),(#13628,#13629,
#13630,#13631),(#13632,#13633,#13634,#13635)),.UNSPECIFIED.,.F.,.F.,.F.,
(4,1,4),(4,4),(0.,0.571428571428571,1.),(-0.00506942997988007,0.618764321025346),
 .UNSPECIFIED.);
#152=B_SPLINE_SURFACE_WITH_KNOTS('',3,3,((#13644,#13645,#13646,#13647,#13648),
(#13649,#13650,#13651,#13652,#13653),(#13654,#13655,#13656,#13657,#13658),
(#13659,#13660,#13661,#13662,#13663),(#13664,#13665,#13666,#13667,#13668)),
 .UNSPECIFIED.,.F.,.F.,.F.,(4,1,4),(4,1,4),(0.,0.571428571428571,1.),(0.244984789862841,
5.12127407770751,11.6229931281671),.UNSPECIFIED.);
#153=B_SPLINE_SURFACE_WITH_KNOTS('',3,3,((#13679,#13680,#13681,#13682),
(#13683,#13684,#13685,#13686),(#13687,#13688,#13689,#13690),(#13691,#13692,
#13693,#13694),(#13695,#13696,#13697,#13698)),.UNSPECIFIED.,.F.,.F.,.F.,
(4,1,4),(4,4),(0.,0.571428571428571,1.),(-0.00403278922781227,0.619909717328002),
 .UNSPECIFIED.);
#154=B_SPLINE_SURFACE_WITH_KNOTS('',3,3,((#13707,#13708,#13709,#13710),
(#13711,#13712,#13713,#13714),(#13715,#13716,#13717,#13718),(#13719,#13720,
#13721,#13722)),.UNSPECIFIED.,.F.,.F.,.F.,(4,4),(4,4),(0.0225340877622934,
0.979701609653785),(0.,0.686930956013783),.UNSPECIFIED.);
#155=B_SPLINE_SURFACE_WITH_KNOTS('',3,3,((#13725,#13726,#13727,#13728),
(#13729,#13730,#13731,#13732),(#13733,#13734,#13735,#13736),(#13737,#13738,
#13739,#13740)),.UNSPECIFIED.,.F.,.F.,.F.,(4,4),(4,4),(0.0202983903462145,
0.977465912237707),(0.,0.686930956013783),.UNSPECIFIED.);
#156=B_SPLINE_SURFACE_WITH_KNOTS('',3,3,((#13811,#13812,#13813,#13814,#13815),
(#13816,#13817,#13818,#13819,#13820),(#13821,#13822,#13823,#13824,#13825),
(#13826,#13827,#13828,#13829,#13830),(#13831,#13832,#13833,#13834,#13835)),
 .UNSPECIFIED.,.F.,.F.,.F.,(4,1,4),(4,1,4),(0.,0.571428571428571,1.),(0.,
0.0439228984074713,0.102486762950766),.UNSPECIFIED.);
#157=B_SPLINE_SURFACE_WITH_KNOTS('',3,3,((#13858,#13859,#13860,#13861,#13862),
(#13863,#13864,#13865,#13866,#13867),(#13868,#13869,#13870,#13871,#13872),
(#13873,#13874,#13875,#13876,#13877),(#13878,#13879,#13880,#13881,#13882)),
 .UNSPECIFIED.,.F.,.F.,.F.,(4,1,4),(4,1,4),(0.,0.571428571428571,1.),(0.,
0.0439228984484775,0.102486763046448),.UNSPECIFIED.);
#158=B_SPLINE_SURFACE_WITH_KNOTS('',3,3,((#13896,#13897,#13898,#13899,#13900,
#13901),(#13902,#13903,#13904,#13905,#13906,#13907),(#13908,#13909,#13910,
#13911,#13912,#13913),(#13914,#13915,#13916,#13917,#13918,#13919),(#13920,
#13921,#13922,#13923,#13924,#13925)),.UNSPECIFIED.,.F.,.F.,.F.,(4,1,4),
(4,1,1,4),(0.,0.571428571428571,1.),(0.,4.74079765360458,7.9013294226743,
11.061861191744),.UNSPECIFIED.);
#159=B_SPLINE_SURFACE_WITH_KNOTS('',3,3,((#13941,#13942,#13943,#13944,#13945),
(#13946,#13947,#13948,#13949,#13950),(#13951,#13952,#13953,#13954,#13955),
(#13956,#13957,#13958,#13959,#13960),(#13961,#13962,#13963,#13964,#13965)),
 .UNSPECIFIED.,.F.,.F.,.F.,(4,1,4),(4,1,4),(0.,0.571428571428571,1.),(0.,
0.0409389169025732,0.0955241394393374),.UNSPECIFIED.);
#160=B_SPLINE_SURFACE_WITH_KNOTS('',3,3,((#13985,#13986,#13987,#13988,#13989),
(#13990,#13991,#13992,#13993,#13994),(#13995,#13996,#13997,#13998,#13999),
(#14000,#14001,#14002,#14003,#14004),(#14005,#14006,#14007,#14008,#14009)),
 .UNSPECIFIED.,.F.,.F.,.F.,(4,1,4),(4,1,4),(0.,0.571428571428571,1.),(2.31010434703409E-17,
0.054585222365383,0.0955241391394202),.UNSPECIFIED.);
#161=B_SPLINE_SURFACE_WITH_KNOTS('',3,3,((#14023,#14024,#14025,#14026,#14027,
#14028),(#14029,#14030,#14031,#14032,#14033,#14034),(#14035,#14036,#14037,
#14038,#14039,#14040),(#14041,#14042,#14043,#14044,#14045,#14046),(#14047,
#14048,#14049,#14050,#14051,#14052)),.UNSPECIFIED.,.F.,.F.,.F.,(4,1,4),
(4,1,1,4),(0.,0.571428571428571,1.),(1.48308270761676E-15,3.16052629084276,
6.32105258168553,11.0618420179497),.UNSPECIFIED.);
#162=B_SPLINE_SURFACE_WITH_KNOTS('',3,3,((#14077,#14078,#14079,#14080),
(#14081,#14082,#14083,#14084),(#14085,#14086,#14087,#14088),(#14089,#14090,
#14091,#14092),(#14093,#14094,#14095,#14096)),.UNSPECIFIED.,.F.,.F.,.F.,
(4,1,4),(4,4),(0.,0.571428571428571,1.),(-0.0018994230917637,0.12591792480537),
 .UNSPECIFIED.);
#163=B_SPLINE_SURFACE_WITH_KNOTS('',3,3,((#14127,#14128,#14129,#14130),
(#14131,#14132,#14133,#14134),(#14135,#14136,#14137,#14138),(#14139,#14140,
#14141,#14142)),.UNSPECIFIED.,.F.,.F.,.F.,(4,4),(4,4),(0.0105624938889701,
0.988135278219398),(0.,0.624639504152193),.UNSPECIFIED.);
#164=B_SPLINE_SURFACE_WITH_KNOTS('',3,3,((#14152,#14153,#14154,#14155),
(#14156,#14157,#14158,#14159),(#14160,#14161,#14162,#14163),(#14164,#14165,
#14166,#14167),(#14168,#14169,#14170,#14171)),.UNSPECIFIED.,.F.,.F.,.F.,
(4,1,4),(4,4),(0.,0.571428571428571,1.),(-0.00248141748936713,0.125282751535517),
 .UNSPECIFIED.);
#165=B_SPLINE_SURFACE_WITH_KNOTS('',3,3,((#14213,#14214,#14215,#14216),
(#14217,#14218,#14219,#14220),(#14221,#14222,#14223,#14224),(#14225,#14226,
#14227,#14228),(#14229,#14230,#14231,#14232)),.UNSPECIFIED.,.F.,.F.,.F.,
(4,1,4),(4,4),(0.,0.571428571428571,1.),(-0.00183337806924316,0.12591792480537),
 .UNSPECIFIED.);
#166=B_SPLINE_SURFACE_WITH_KNOTS('',3,3,((#14263,#14264,#14265,#14266),
(#14267,#14268,#14269,#14270),(#14271,#14272,#14273,#14274),(#14275,#14276,
#14277,#14278),(#14279,#14280,#14281,#14282)),.UNSPECIFIED.,.F.,.F.,.F.,
(4,1,4),(4,4),(0.,0.571428571428571,1.),(-0.00256306836558615,0.125282751535516),
 .UNSPECIFIED.);
#167=B_SPLINE_SURFACE_WITH_KNOTS('',3,3,((#14321,#14322,#14323,#14324),
(#14325,#14326,#14327,#14328),(#14329,#14330,#14331,#14332),(#14333,#14334,
#14335,#14336)),.UNSPECIFIED.,.F.,.F.,.F.,(4,4),(4,4),(0.0118647217806023,
0.98943750611103),(0.,0.624639504152185),.UNSPECIFIED.);
#168=B_SPLINE_SURFACE_WITH_KNOTS('',3,3,((#16719,#16720,#16721,#16722,#16723,
#16724,#16725,#16726,#16727,#16728,#16729,#16730,#16731,#16732,#16733,#16734,
#16735,#16736,#16737,#16738,#16739,#16740,#16741,#16742,#16743,#16744,#16745,
#16746,#16747,#16748,#16749,#16750,#16751,#16752,#16753,#16754,#16755,#16756,
#16757,#16758,#16759,#16760,#16761,#16762,#16763,#16764,#16765,#16766,#16767,
#16768,#16769,#16770,#16771,#16772,#16773,#16774,#16775,#16776,#16777,#16778,
#16779,#16780,#16781,#16782,#16783,#16784,#16785,#16786,#16787,#16788,#16789,
#16790,#16791,#16792,#16793,#16794,#16795,#16796,#16797,#16798,#16799,#16800,
#16801,#16802,#16803,#16804,#16805,#16806,#16807,#16808,#16809,#16810,#16811,
#16812,#16813,#16814,#16815,#16816,#16817,#16818,#16819,#16820,#16821,#16822,
#16823,#16824,#16825,#16826,#16827,#16828,#16829,#16830,#16831,#16832,#16833,
#16834,#16835,#16836,#16837,#16838,#16839,#16840,#16841,#16842,#16843,#16844,
#16845,#16846,#16847,#16848,#16849,#16850,#16851,#16852,#16853,#16854,#16855,
#16856,#16857,#16858,#16859,#16860,#16861,#16862,#16863,#16864,#16865,#16866,
#16867,#16868,#16869,#16870,#16871,#16872,#16873,#16874,#16875,#16876,#16877,
#16878,#16879,#16880,#16881,#16882,#16883,#16884,#16885,#16886,#16887,#16888,
#16889,#16890,#16891,#16892,#16893,#16894,#16895,#16896,#16897,#16898,#16899,
#16900,#16901,#16902,#16903,#16904,#16905,#16906,#16907,#16908,#16909,#16910,
#16911,#16912,#16913,#16914),(#16915,#16916,#16917,#16918,#16919,#16920,
#16921,#16922,#16923,#16924,#16925,#16926,#16927,#16928,#16929,#16930,#16931,
#16932,#16933,#16934,#16935,#16936,#16937,#16938,#16939,#16940,#16941,#16942,
#16943,#16944,#16945,#16946,#16947,#16948,#16949,#16950,#16951,#16952,#16953,
#16954,#16955,#16956,#16957,#16958,#16959,#16960,#16961,#16962,#16963,#16964,
#16965,#16966,#16967,#16968,#16969,#16970,#16971,#16972,#16973,#16974,#16975,
#16976,#16977,#16978,#16979,#16980,#16981,#16982,#16983,#16984,#16985,#16986,
#16987,#16988,#16989,#16990,#16991,#16992,#16993,#16994,#16995,#16996,#16997,
#16998,#16999,#17000,#17001,#17002,#17003,#17004,#17005,#17006,#17007,#17008,
#17009,#17010,#17011,#17012,#17013,#17014,#17015,#17016,#17017,#17018,#17019,
#17020,#17021,#17022,#17023,#17024,#17025,#17026,#17027,#17028,#17029,#17030,
#17031,#17032,#17033,#17034,#17035,#17036,#17037,#17038,#17039,#17040,#17041,
#17042,#17043,#17044,#17045,#17046,#17047,#17048,#17049,#17050,#17051,#17052,
#17053,#17054,#17055,#17056,#17057,#17058,#17059,#17060,#17061,#17062,#17063,
#17064,#17065,#17066,#17067,#17068,#17069,#17070,#17071,#17072,#17073,#17074,
#17075,#17076,#17077,#17078,#17079,#17080,#17081,#17082,#17083,#17084,#17085,
#17086,#17087,#17088,#17089,#17090,#17091,#17092,#17093,#17094,#17095,#17096,
#17097,#17098,#17099,#17100,#17101,#17102,#17103,#17104,#17105,#17106,#17107,
#17108,#17109,#17110),(#17111,#17112,#17113,#17114,#17115,#17116,#17117,
#17118,#17119,#17120,#17121,#17122,#17123,#17124,#17125,#17126,#17127,#17128,
#17129,#17130,#17131,#17132,#17133,#17134,#17135,#17136,#17137,#17138,#17139,
#17140,#17141,#17142,#17143,#17144,#17145,#17146,#17147,#17148,#17149,#17150,
#17151,#17152,#17153,#17154,#17155,#17156,#17157,#17158,#17159,#17160,#17161,
#17162,#17163,#17164,#17165,#17166,#17167,#17168,#17169,#17170,#17171,#17172,
#17173,#17174,#17175,#17176,#17177,#17178,#17179,#17180,#17181,#17182,#17183,
#17184,#17185,#17186,#17187,#17188,#17189,#17190,#17191,#17192,#17193,#17194,
#17195,#17196,#17197,#17198,#17199,#17200,#17201,#17202,#17203,#17204,#17205,
#17206,#17207,#17208,#17209,#17210,#17211,#17212,#17213,#17214,#17215,#17216,
#17217,#17218,#17219,#17220,#17221,#17222,#17223,#17224,#17225,#17226,#17227,
#17228,#17229,#17230,#17231,#17232,#17233,#17234,#17235,#17236,#17237,#17238,
#17239,#17240,#17241,#17242,#17243,#17244,#17245,#17246,#17247,#17248,#17249,
#17250,#17251,#17252,#17253,#17254,#17255,#17256,#17257,#17258,#17259,#17260,
#17261,#17262,#17263,#17264,#17265,#17266,#17267,#17268,#17269,#17270,#17271,
#17272,#17273,#17274,#17275,#17276,#17277,#17278,#17279,#17280,#17281,#17282,
#17283,#17284,#17285,#17286,#17287,#17288,#17289,#17290,#17291,#17292,#17293,
#17294,#17295,#17296,#17297,#17298,#17299,#17300,#17301,#17302,#17303,#17304,
#17305,#17306),(#17307,#17308,#17309,#17310,#17311,#17312,#17313,#17314,
#17315,#17316,#17317,#17318,#17319,#17320,#17321,#17322,#17323,#17324,#17325,
#17326,#17327,#17328,#17329,#17330,#17331,#17332,#17333,#17334,#17335,#17336,
#17337,#17338,#17339,#17340,#17341,#17342,#17343,#17344,#17345,#17346,#17347,
#17348,#17349,#17350,#17351,#17352,#17353,#17354,#17355,#17356,#17357,#17358,
#17359,#17360,#17361,#17362,#17363,#17364,#17365,#17366,#17367,#17368,#17369,
#17370,#17371,#17372,#17373,#17374,#17375,#17376,#17377,#17378,#17379,#17380,
#17381,#17382,#17383,#17384,#17385,#17386,#17387,#17388,#17389,#17390,#17391,
#17392,#17393,#17394,#17395,#17396,#17397,#17398,#17399,#17400,#17401,#17402,
#17403,#17404,#17405,#17406,#17407,#17408,#17409,#17410,#17411,#17412,#17413,
#17414,#17415,#17416,#17417,#17418,#17419,#17420,#17421,#17422,#17423,#17424,
#17425,#17426,#17427,#17428,#17429,#17430,#17431,#17432,#17433,#17434,#17435,
#17436,#17437,#17438,#17439,#17440,#17441,#17442,#17443,#17444,#17445,#17446,
#17447,#17448,#17449,#17450,#17451,#17452,#17453,#17454,#17455,#17456,#17457,
#17458,#17459,#17460,#17461,#17462,#17463,#17464,#17465,#17466,#17467,#17468,
#17469,#17470,#17471,#17472,#17473,#17474,#17475,#17476,#17477,#17478,#17479,
#17480,#17481,#17482,#17483,#17484,#17485,#17486,#17487,#17488,#17489,#17490,
#17491,#17492,#17493,#17494,#17495,#17496,#17497,#17498,#17499,#17500,#17501,
#17502)),.UNSPECIFIED.,.F.,.F.,.F.,(4,4),(4,1,1,1,1,1,1,1,1,1,1,1,1,1,1,
1,1,1,1,1,1,1,1,1,1,1,1,1,1,1,1,1,1,1,1,1,1,1,1,1,1,1,1,1,1,1,1,1,1,1,1,
1,1,1,1,1,1,1,1,1,1,1,1,1,1,1,1,1,1,1,1,1,1,1,1,1,1,1,1,1,1,1,1,1,1,1,1,
1,1,1,1,1,1,1,1,1,1,1,1,1,1,1,1,1,1,1,1,1,1,1,1,1,1,1,1,1,1,1,1,1,1,1,1,
1,1,1,1,1,1,1,1,1,1,1,1,1,1,1,1,1,1,1,1,1,1,1,1,1,1,1,1,1,1,1,1,1,1,1,1,
1,1,1,1,1,1,1,1,1,1,1,1,1,1,1,1,1,1,1,1,1,1,1,1,1,1,1,1,1,1,1,1,1,1,4),
(0.,0.0329955678841871),(11.6159397475006,12.61358260836,13.6112254692194,
14.6088683300789,15.6065111909383,16.6041540517977,17.6017969126571,18.5994397735165,
19.5970826343759,20.5947254952353,21.5923683560947,22.5900112169541,23.5876540778135,
24.5852969386729,25.5829397995323,26.5805826603917,27.5782255212511,28.5758683821105,
29.5735112429699,30.5711541038294,31.5687969646888,32.5664398255482,33.5640826864076,
34.561725547267,35.5593684081264,36.5570112689858,37.5546541298452,38.5522969907046,
39.549939851564,40.5475827124234,41.5452255732828,42.5428684341422,43.5405112950016,
44.538154155861,45.5357970167204,46.5334398775799,47.5310827384393,48.5287255992987,
49.5263684601581,50.5240113210175,51.5216541818769,52.5192970427363,53.5169399035957,
54.5145827644551,55.5122256253145,56.5098684861739,57.5075113470333,58.5051542078927,
59.5027970687521,60.5004399296115,61.4980827904709,62.4957256513303,63.4933685121897,
64.4910113730492,65.4886542339086,66.486297094768,67.4839399556274,68.4815828164868,
69.4792256773462,70.4768685382056,71.474511399065,72.4721542599244,73.4697971207838,
74.4674399816432,75.4650828425026,76.462725703362,77.4603685642214,78.4580114250808,
79.4556542859402,80.4532971467996,81.4509400076591,82.4485828685185,83.4462257293779,
84.4438685902373,85.4415114510967,86.4391543119561,87.4367971728155,88.4344400336749,
89.4320828945343,90.4297257553937,91.4273686162531,92.4250114771125,93.4226543379719,
94.4202971988313,95.4179400596907,96.4155829205502,97.4132257814096,98.410868642269,
99.4085115031284,100.406154363988,101.403797224847,102.401440085707,103.399082946566,
104.396725807425,105.394368668285,106.392011529144,107.389654390004,108.387297250863,
109.384940111722,110.382582972582,111.380225833441,112.377868694301,113.37551155516,
114.373154416019,115.370797276879,116.368440137738,117.366082998598,118.363725859457,
119.361368720316,120.359011581176,121.356654442035,122.354297302895,123.351940163754,
124.349583024614,125.347225885473,126.344868746332,127.342511607192,128.340154468051,
129.337797328911,130.33544018977,131.333083050629,132.330725911489,133.328368772348,
134.326011633208,135.323654494067,136.321297354926,137.318940215786,138.316583076645,
139.314225937505,140.311868798364,141.309511659223,142.307154520083,143.304797380942,
144.302440241802,145.300083102661,146.29772596352,147.29536882438,148.293011685239,
149.290654546099,150.288297406958,151.285940267817,152.283583128677,153.281225989536,
154.278868850396,155.276511711255,156.274154572115,157.271797432974,158.269440293833,
159.267083154693,160.264726015552,161.262368876412,162.260011737271,163.25765459813,
164.25529745899,165.252940319849,166.250583180709,167.248226041568,168.245868902427,
169.243511763287,170.241154624146,171.238797485006,172.236440345865,173.234083206724,
174.231726067584,175.229368928443,176.227011789303,177.224654650162,178.222297511021,
179.219940371881,180.21758323274,181.2152260936,182.212868954459,183.210511815318,
184.208154676178,185.205797537037,186.203440397897,187.201083258756,188.198726119616,
189.196368980475,190.194011841334,191.191654702194,192.189297563053,193.186940423913,
194.184583284772,195.182226145631,196.179869006491,197.17751186735,198.17515472821,
199.172797589069,200.170440449928,201.168083310788,202.165726171647,203.163369032507,
204.161011893366),.UNSPECIFIED.);
#169=B_SPLINE_SURFACE_WITH_KNOTS('',3,3,((#17592,#17593,#17594,#17595,#17596,
#17597,#17598,#17599,#17600,#17601,#17602,#17603,#17604,#17605,#17606,#17607,
#17608,#17609,#17610,#17611,#17612,#17613,#17614,#17615,#17616,#17617,#17618,
#17619,#17620,#17621,#17622,#17623,#17624,#17625,#17626,#17627,#17628,#17629,
#17630,#17631,#17632,#17633,#17634,#17635,#17636,#17637,#17638,#17639,#17640,
#17641,#17642,#17643,#17644,#17645,#17646,#17647,#17648,#17649,#17650,#17651,
#17652,#17653,#17654,#17655,#17656,#17657,#17658,#17659,#17660,#17661,#17662,
#17663,#17664,#17665,#17666,#17667,#17668,#17669,#17670,#17671,#17672,#17673,
#17674,#17675,#17676,#17677,#17678,#17679,#17680,#17681,#17682,#17683,#17684,
#17685,#17686,#17687,#17688,#17689,#17690,#17691,#17692,#17693,#17694,#17695,
#17696,#17697,#17698,#17699,#17700,#17701,#17702,#17703,#17704,#17705,#17706,
#17707,#17708,#17709,#17710,#17711,#17712,#17713,#17714,#17715,#17716,#17717,
#17718,#17719,#17720,#17721,#17722,#17723,#17724,#17725,#17726,#17727,#17728,
#17729,#17730,#17731,#17732,#17733,#17734,#17735,#17736,#17737,#17738,#17739,
#17740,#17741,#17742,#17743,#17744,#17745,#17746,#17747,#17748,#17749,#17750,
#17751,#17752,#17753,#17754,#17755,#17756,#17757,#17758,#17759,#17760,#17761,
#17762,#17763,#17764,#17765,#17766,#17767,#17768,#17769,#17770,#17771,#17772,
#17773,#17774,#17775,#17776,#17777,#17778,#17779,#17780,#17781,#17782,#17783,
#17784,#17785,#17786,#17787,#17788,#17789),(#17790,#17791,#17792,#17793,
#17794,#17795,#17796,#17797,#17798,#17799,#17800,#17801,#17802,#17803,#17804,
#17805,#17806,#17807,#17808,#17809,#17810,#17811,#17812,#17813,#17814,#17815,
#17816,#17817,#17818,#17819,#17820,#17821,#17822,#17823,#17824,#17825,#17826,
#17827,#17828,#17829,#17830,#17831,#17832,#17833,#17834,#17835,#17836,#17837,
#17838,#17839,#17840,#17841,#17842,#17843,#17844,#17845,#17846,#17847,#17848,
#17849,#17850,#17851,#17852,#17853,#17854,#17855,#17856,#17857,#17858,#17859,
#17860,#17861,#17862,#17863,#17864,#17865,#17866,#17867,#17868,#17869,#17870,
#17871,#17872,#17873,#17874,#17875,#17876,#17877,#17878,#17879,#17880,#17881,
#17882,#17883,#17884,#17885,#17886,#17887,#17888,#17889,#17890,#17891,#17892,
#17893,#17894,#17895,#17896,#17897,#17898,#17899,#17900,#17901,#17902,#17903,
#17904,#17905,#17906,#17907,#17908,#17909,#17910,#17911,#17912,#17913,#17914,
#17915,#17916,#17917,#17918,#17919,#17920,#17921,#17922,#17923,#17924,#17925,
#17926,#17927,#17928,#17929,#17930,#17931,#17932,#17933,#17934,#17935,#17936,
#17937,#17938,#17939,#17940,#17941,#17942,#17943,#17944,#17945,#17946,#17947,
#17948,#17949,#17950,#17951,#17952,#17953,#17954,#17955,#17956,#17957,#17958,
#17959,#17960,#17961,#17962,#17963,#17964,#17965,#17966,#17967,#17968,#17969,
#17970,#17971,#17972,#17973,#17974,#17975,#17976,#17977,#17978,#17979,#17980,
#17981,#17982,#17983,#17984,#17985,#17986,#17987),(#17988,#17989,#17990,
#17991,#17992,#17993,#17994,#17995,#17996,#17997,#17998,#17999,#18000,#18001,
#18002,#18003,#18004,#18005,#18006,#18007,#18008,#18009,#18010,#18011,#18012,
#18013,#18014,#18015,#18016,#18017,#18018,#18019,#18020,#18021,#18022,#18023,
#18024,#18025,#18026,#18027,#18028,#18029,#18030,#18031,#18032,#18033,#18034,
#18035,#18036,#18037,#18038,#18039,#18040,#18041,#18042,#18043,#18044,#18045,
#18046,#18047,#18048,#18049,#18050,#18051,#18052,#18053,#18054,#18055,#18056,
#18057,#18058,#18059,#18060,#18061,#18062,#18063,#18064,#18065,#18066,#18067,
#18068,#18069,#18070,#18071,#18072,#18073,#18074,#18075,#18076,#18077,#18078,
#18079,#18080,#18081,#18082,#18083,#18084,#18085,#18086,#18087,#18088,#18089,
#18090,#18091,#18092,#18093,#18094,#18095,#18096,#18097,#18098,#18099,#18100,
#18101,#18102,#18103,#18104,#18105,#18106,#18107,#18108,#18109,#18110,#18111,
#18112,#18113,#18114,#18115,#18116,#18117,#18118,#18119,#18120,#18121,#18122,
#18123,#18124,#18125,#18126,#18127,#18128,#18129,#18130,#18131,#18132,#18133,
#18134,#18135,#18136,#18137,#18138,#18139,#18140,#18141,#18142,#18143,#18144,
#18145,#18146,#18147,#18148,#18149,#18150,#18151,#18152,#18153,#18154,#18155,
#18156,#18157,#18158,#18159,#18160,#18161,#18162,#18163,#18164,#18165,#18166,
#18167,#18168,#18169,#18170,#18171,#18172,#18173,#18174,#18175,#18176,#18177,
#18178,#18179,#18180,#18181,#18182,#18183,#18184,#18185),(#18186,#18187,
#18188,#18189,#18190,#18191,#18192,#18193,#18194,#18195,#18196,#18197,#18198,
#18199,#18200,#18201,#18202,#18203,#18204,#18205,#18206,#18207,#18208,#18209,
#18210,#18211,#18212,#18213,#18214,#18215,#18216,#18217,#18218,#18219,#18220,
#18221,#18222,#18223,#18224,#18225,#18226,#18227,#18228,#18229,#18230,#18231,
#18232,#18233,#18234,#18235,#18236,#18237,#18238,#18239,#18240,#18241,#18242,
#18243,#18244,#18245,#18246,#18247,#18248,#18249,#18250,#18251,#18252,#18253,
#18254,#18255,#18256,#18257,#18258,#18259,#18260,#18261,#18262,#18263,#18264,
#18265,#18266,#18267,#18268,#18269,#18270,#18271,#18272,#18273,#18274,#18275,
#18276,#18277,#18278,#18279,#18280,#18281,#18282,#18283,#18284,#18285,#18286,
#18287,#18288,#18289,#18290,#18291,#18292,#18293,#18294,#18295,#18296,#18297,
#18298,#18299,#18300,#18301,#18302,#18303,#18304,#18305,#18306,#18307,#18308,
#18309,#18310,#18311,#18312,#18313,#18314,#18315,#18316,#18317,#18318,#18319,
#18320,#18321,#18322,#18323,#18324,#18325,#18326,#18327,#18328,#18329,#18330,
#18331,#18332,#18333,#18334,#18335,#18336,#18337,#18338,#18339,#18340,#18341,
#18342,#18343,#18344,#18345,#18346,#18347,#18348,#18349,#18350,#18351,#18352,
#18353,#18354,#18355,#18356,#18357,#18358,#18359,#18360,#18361,#18362,#18363,
#18364,#18365,#18366,#18367,#18368,#18369,#18370,#18371,#18372,#18373,#18374,
#18375,#18376,#18377,#18378,#18379,#18380,#18381,#18382,#18383)),
 .UNSPECIFIED.,.F.,.F.,.F.,(4,4),(4,1,1,1,1,1,1,1,1,1,1,1,1,1,1,1,1,1,1,
1,1,1,1,1,1,1,1,1,1,1,1,1,1,1,1,1,1,1,1,1,1,1,1,1,1,1,1,1,1,1,1,1,1,1,1,
1,1,1,1,1,1,1,1,1,1,1,1,1,1,1,1,1,1,1,1,1,1,1,1,1,1,1,1,1,1,1,1,1,1,1,1,
1,1,1,1,1,1,1,1,1,1,1,1,1,1,1,1,1,1,1,1,1,1,1,1,1,1,1,1,1,1,1,1,1,1,1,1,
1,1,1,1,1,1,1,1,1,1,1,1,1,1,1,1,1,1,1,1,1,1,1,1,1,1,1,1,1,1,1,1,1,1,1,1,
1,1,1,1,1,1,1,1,1,1,1,1,1,1,1,1,1,1,1,1,1,1,1,1,1,1,1,1,1,1,1,1,4),(0.,
0.0329955678841871),(8.30203615430855,9.30007843543257,10.2981207165566,
11.2961629976806,12.2942052788047,13.2922475599287,14.2902898410527,15.2883321221767,
16.2863744033008,17.2844166844248,18.2824589655488,19.2805012466728,20.2785435277969,
21.2765858089209,22.2746280900449,23.272670371169,24.270712652293,25.268754933417,
26.266797214541,27.2648394956651,28.2628817767891,29.2609240579131,30.2589663390371,
31.2570086201612,32.2550509012852,33.2530931824092,34.2511354635333,35.2491777446573,
36.2472200257813,37.2452623069053,38.2433045880294,39.2413468691534,40.2393891502774,
41.2374314314014,42.2354737125255,43.2335159936495,44.2315582747735,45.2296005558975,
46.2276428370216,47.2256851181456,48.2237273992696,49.2217696803937,50.2198119615177,
51.2178542426417,52.2158965237657,53.2139388048898,54.2119810860138,55.2100233671378,
56.2080656482619,57.2061079293859,58.2041502105099,59.2021924916339,60.200234772758,
61.198277053882,62.196319335006,63.19436161613,64.1924038972541,65.1904461783781,
66.1884884595021,67.1865307406262,68.1845730217502,69.1826153028742,70.1806575839982,
71.1786998651223,72.1767421462463,73.1747844273703,74.1728267084943,75.1708689896184,
76.1689112707424,77.1669535518664,78.1649958329905,79.1630381141145,80.1610803952385,
81.1591226763625,82.1571649574865,83.1552072386106,84.1532495197346,85.1512918008586,
86.1493340819827,87.1473763631067,88.1454186442307,89.1434609253548,90.1415032064788,
91.1395454876028,92.1375877687268,93.1356300498508,94.1336723309749,95.1317146120989,
96.1297568932229,97.127799174347,98.125841455471,99.123883736595,100.121926017719,
101.119968298843,102.118010579967,103.116052861091,104.114095142215,105.112137423339,
106.110179704463,107.108221985587,108.106264266711,109.104306547835,110.102348828959,
111.100391110083,112.098433391207,113.096475672331,114.094517953455,115.092560234579,
116.090602515703,117.088644796828,118.086687077952,119.084729359076,120.0827716402,
121.080813921324,122.078856202448,123.076898483572,124.074940764696,125.07298304582,
126.071025326944,127.069067608068,128.067109889192,129.065152170316,130.06319445144,
131.061236732564,132.059279013688,133.057321294812,134.055363575936,135.05340585706,
136.051448138184,137.049490419308,138.047532700432,139.045574981556,140.04361726268,
141.041659543804,142.039701824928,143.037744106052,144.035786387176,145.0338286683,
146.031870949424,147.029913230548,148.027955511672,149.025997792796,150.02404007392,
151.022082355044,152.020124636168,153.018166917292,154.016209198417,155.014251479541,
156.012293760665,157.010336041789,158.008378322913,159.006420604037,160.004462885161,
161.002505166285,162.000547447409,162.998589728533,163.996632009657,164.994674290781,
165.992716571905,166.990758853029,167.988801134153,168.986843415277,169.984885696401,
170.982927977525,171.980970258649,172.979012539773,173.977054820897,174.975097102021,
175.973139383145,176.971181664269,177.969223945393,178.967266226517,179.965308507641,
180.963350788765,181.961393069889,182.959435351013,183.957477632137,184.955519913261,
185.953562194385,186.951604475509,187.949646756633,188.947689037757,189.945731318881,
190.943773600006,191.94181588113,192.939858162254,193.937900443378,194.935942724502,
195.933985005626,196.93202728675,197.930069567874,198.928111848998,199.926154130122,
200.924196411246,201.92223869237,202.920280973494),.UNSPECIFIED.);
#170=B_SPLINE_SURFACE_WITH_KNOTS('',3,3,((#18842,#18843,#18844,#18845,#18846,
#18847,#18848,#18849,#18850,#18851,#18852,#18853,#18854,#18855,#18856,#18857,
#18858,#18859,#18860,#18861,#18862,#18863,#18864,#18865,#18866,#18867,#18868,
#18869,#18870,#18871,#18872,#18873,#18874,#18875,#18876,#18877),(#18878,
#18879,#18880,#18881,#18882,#18883,#18884,#18885,#18886,#18887,#18888,#18889,
#18890,#18891,#18892,#18893,#18894,#18895,#18896,#18897,#18898,#18899,#18900,
#18901,#18902,#18903,#18904,#18905,#18906,#18907,#18908,#18909,#18910,#18911,
#18912,#18913),(#18914,#18915,#18916,#18917,#18918,#18919,#18920,#18921,
#18922,#18923,#18924,#18925,#18926,#18927,#18928,#18929,#18930,#18931,#18932,
#18933,#18934,#18935,#18936,#18937,#18938,#18939,#18940,#18941,#18942,#18943,
#18944,#18945,#18946,#18947,#18948,#18949),(#18950,#18951,#18952,#18953,
#18954,#18955,#18956,#18957,#18958,#18959,#18960,#18961,#18962,#18963,#18964,
#18965,#18966,#18967,#18968,#18969,#18970,#18971,#18972,#18973,#18974,#18975,
#18976,#18977,#18978,#18979,#18980,#18981,#18982,#18983,#18984,#18985)),
 .UNSPECIFIED.,.F.,.F.,.F.,(4,4),(4,1,1,1,1,1,1,1,1,1,1,1,1,1,1,1,1,1,1,
1,1,1,1,1,1,1,1,1,1,1,1,1,1,4),(0.,0.0321584099938622),(11.8553612635794,
12.830508595889,13.8056559281987,14.7808032605084,15.755950592818,16.7310979251277,
17.7062452574374,18.681392589747,19.6565399220567,20.6316872543664,21.606834586676,
22.5819819189857,23.5571292512954,24.532276583605,25.5074239159147,26.4825712482243,
27.457718580534,28.4328659128437,29.4080132451533,30.383160577463,31.3583079097727,
32.3334552420823,33.308602574392,34.2837499067017,35.2588972390113,36.234044571321,
37.2091919036307,38.1843392359403,39.15948656825,40.1346339005596,41.1097812328693,
42.084928565179,43.0600758974886,44.0352232297983),.UNSPECIFIED.);
#171=B_SPLINE_SURFACE_WITH_KNOTS('',3,3,((#19109,#19110,#19111,#19112,#19113,
#19114,#19115,#19116,#19117,#19118,#19119,#19120,#19121,#19122,#19123,#19124,
#19125,#19126,#19127,#19128,#19129,#19130,#19131,#19132,#19133,#19134,#19135,
#19136,#19137,#19138,#19139,#19140,#19141,#19142,#19143,#19144),(#19145,
#19146,#19147,#19148,#19149,#19150,#19151,#19152,#19153,#19154,#19155,#19156,
#19157,#19158,#19159,#19160,#19161,#19162,#19163,#19164,#19165,#19166,#19167,
#19168,#19169,#19170,#19171,#19172,#19173,#19174,#19175,#19176,#19177,#19178,
#19179,#19180),(#19181,#19182,#19183,#19184,#19185,#19186,#19187,#19188,
#19189,#19190,#19191,#19192,#19193,#19194,#19195,#19196,#19197,#19198,#19199,
#19200,#19201,#19202,#19203,#19204,#19205,#19206,#19207,#19208,#19209,#19210,
#19211,#19212,#19213,#19214,#19215,#19216),(#19217,#19218,#19219,#19220,
#19221,#19222,#19223,#19224,#19225,#19226,#19227,#19228,#19229,#19230,#19231,
#19232,#19233,#19234,#19235,#19236,#19237,#19238,#19239,#19240,#19241,#19242,
#19243,#19244,#19245,#19246,#19247,#19248,#19249,#19250,#19251,#19252)),
 .UNSPECIFIED.,.F.,.F.,.F.,(4,4),(4,1,1,1,1,1,1,1,1,1,1,1,1,1,1,1,1,1,1,
1,1,1,1,1,1,1,1,1,1,1,1,1,1,4),(0.,0.0321584099938622),(14.3984001269719,
15.3735474592815,16.3486947915912,17.3238421239009,18.2989894562105,19.2741367885202,
20.2492841208299,21.2244314531395,22.1995787854492,23.1747261177589,24.1498734500685,
25.1250207823782,26.1001681146879,27.0753154469975,28.0504627793072,29.0256101116168,
30.0007574439265,30.9759047762362,31.9510521085458,32.9261994408555,33.9013467731652,
34.8764941054748,35.8516414377845,36.8267887700942,37.8019361024038,38.7770834347135,
39.7522307670232,40.7273780993328,41.7025254316425,42.6776727639522,43.6528200962618,
44.6279674285715,45.6031147608811,46.5782620931908),.UNSPECIFIED.);
#172=B_SPLINE_CURVE_WITH_KNOTS('',3,(#9958,#9959,#9960,#9961,#9962,#9963),
 .UNSPECIFIED.,.F.,.F.,(4,2,4),(-0.607240122656937,-0.303691721894415,-0.000634514333697656),
 .UNSPECIFIED.);
#173=B_SPLINE_CURVE_WITH_KNOTS('',3,(#9965,#9966,#9967,#9968,#9969,#9970,
#9971,#9972,#9973,#9974,#9975,#9976,#9977,#9978,#9979,#9980,#9981,#9982,
#9983,#9984,#9985,#9986,#9987,#9988,#9989,#9990,#9991,#9992),
 .UNSPECIFIED.,.F.,.F.,(4,3,3,3,3,3,3,3,3,4),(-0.152223584381152,-0.128403685910756,
-0.115058138924018,-0.0911105876986024,-0.0779275105489685,-0.0651650823668383,
-0.0413494676927402,-0.0389105926748606,-0.0151313403168948,0.),
 .UNSPECIFIED.);
#174=B_SPLINE_CURVE_WITH_KNOTS('',3,(#9996,#9997,#9998,#9999,#10000,#10001,
#10002,#10003,#10004,#10005,#10006,#10007,#10008,#10009,#10010,#10011,#10012,
#10013,#10014,#10015,#10016,#10017,#10018,#10019,#10020,#10021,#10022,#10023),
 .UNSPECIFIED.,.F.,.F.,(4,3,3,3,3,3,3,3,3,4),(-0.152249917238265,-0.128484865669312,
-0.115494642307313,-0.0916985948709881,-0.0870953287403626,-0.0787006597758974,
-0.0547717013112817,-0.0393956522318865,-0.0155460991587222,0.),
 .UNSPECIFIED.);
#175=B_SPLINE_CURVE_WITH_KNOTS('',3,(#10024,#10025,#10026,#10027,#10028,
#10029),.UNSPECIFIED.,.F.,.F.,(4,2,4),(-0.606785315485727,-0.30369188913634,
-0.000179692314978108),.UNSPECIFIED.);
#176=B_SPLINE_CURVE_WITH_KNOTS('',3,(#10034,#10035,#10036,#10037,#10038,
#10039),.UNSPECIFIED.,.F.,.F.,(4,2,4),(-0.606332812995025,-0.303737653350621,
-0.000161665236032726),.UNSPECIFIED.);
#177=B_SPLINE_CURVE_WITH_KNOTS('',3,(#10041,#10042,#10043,#10044,#10045,
#10046,#10047,#10048,#10049,#10050,#10051,#10052,#10053,#10054,#10055,#10056,
#10057,#10058,#10059,#10060,#10061,#10062,#10063,#10064,#10065,#10066,#10067,
#10068),.UNSPECIFIED.,.F.,.F.,(4,3,3,3,3,3,3,3,3,4),(-0.152301160038588,
-0.128555435257278,-0.115184785848022,-0.0912639339035621,-0.0780773216554274,
-0.065267350293706,-0.0414723266145325,-0.0390252168402571,-0.0152374671294611,
0.),.UNSPECIFIED.);
#178=B_SPLINE_CURVE_WITH_KNOTS('',3,(#10072,#10073,#10074,#10075,#10076,
#10077,#10078,#10079,#10080,#10081,#10082,#10083,#10084,#10085,#10086,#10087,
#10088,#10089,#10090,#10091,#10092,#10093,#10094,#10095,#10096,#10097,#10098,
#10099),.UNSPECIFIED.,.F.,.F.,(4,3,3,3,3,3,3,3,3,4),(-0.152307894271445,
-0.128535938708366,-0.115295945509717,-0.0915234088298753,-0.0870575315710991,
-0.0782740392368046,-0.0543664511067997,-0.0391484926712317,-0.0153774171089249,
0.),.UNSPECIFIED.);
#179=B_SPLINE_CURVE_WITH_KNOTS('',3,(#10101,#10102,#10103,#10104,#10105,
#10106),.UNSPECIFIED.,.F.,.F.,(4,2,4),(-0.607315067615316,-0.303737782617996,
-0.00114390098251854),.UNSPECIFIED.);
#180=B_SPLINE_CURVE_WITH_KNOTS('',3,(#10112,#10113,#10114,#10115,#10116,
#10117),.UNSPECIFIED.,.F.,.F.,(4,2,4),(-0.606335618682527,-0.303964064424246,
-0.000163142902895597),.UNSPECIFIED.);
#181=B_SPLINE_CURVE_WITH_KNOTS('',3,(#10119,#10120,#10121,#10122,#10123,
#10124,#10125,#10126,#10127,#10128,#10129,#10130,#10131,#10132,#10133,#10134,
#10135,#10136,#10137,#10138,#10139,#10140,#10141,#10142,#10143,#10144,#10145,
#10146),.UNSPECIFIED.,.F.,.F.,(4,3,3,3,3,3,3,3,3,4),(-0.152324888062519,
-0.128571266282871,-0.115187819092559,-0.0912644922975459,-0.0780623053857969,
-0.0652705430018984,-0.0414736125245103,-0.0390138150290758,-0.015226502089553,
0.),.UNSPECIFIED.);
#182=B_SPLINE_CURVE_WITH_KNOTS('',3,(#10150,#10151,#10152,#10153,#10154,
#10155,#10156,#10157,#10158,#10159,#10160,#10161,#10162,#10163,#10164,#10165,
#10166,#10167,#10168,#10169,#10170,#10171,#10172,#10173,#10174,#10175,#10176,
#10177),.UNSPECIFIED.,.F.,.F.,(4,3,3,3,3,3,3,3,3,4),(-0.152333600285603,
-0.128561769460285,-0.115331525958272,-0.0915566852459163,-0.0870792380259527,
-0.0783165909319309,-0.0544069520497563,-0.0391732033593778,-0.0153939862842036,
0.),.UNSPECIFIED.);
#183=B_SPLINE_CURVE_WITH_KNOTS('',3,(#10179,#10180,#10181,#10182,#10183,
#10184),.UNSPECIFIED.,.F.,.F.,(4,2,4),(-0.607765665607205,-0.303964210965506,
-0.00159316434717749),.UNSPECIFIED.);
#184=B_SPLINE_CURVE_WITH_KNOTS('',3,(#10190,#10191,#10192,#10193,#10194,
#10195),.UNSPECIFIED.,.F.,.F.,(4,2,4),(-0.608113833554089,-0.304405910662044,
-0.00120843896277512),.UNSPECIFIED.);
#185=B_SPLINE_CURVE_WITH_KNOTS('',3,(#10197,#10198,#10199,#10200,#10201,
#10202,#10203,#10204,#10205,#10206,#10207,#10208,#10209,#10210,#10211,#10212,
#10213,#10214,#10215,#10216,#10217,#10218,#10219,#10220,#10221,#10222,#10223,
#10224),.UNSPECIFIED.,.F.,.F.,(4,3,3,3,3,3,3,3,3,4),(-0.152638346832965,
-0.128647829044501,-0.117000727359648,-0.0929750760194364,-0.0775532335837778,
-0.065166230851578,-0.0413072760700971,-0.0386249916896363,-0.0148681833632798,
0.),.UNSPECIFIED.);
#186=B_SPLINE_CURVE_WITH_KNOTS('',3,(#10228,#10229,#10230,#10231,#10232,
#10233,#10234,#10235,#10236,#10237,#10238,#10239,#10240,#10241,#10242,#10243,
#10244,#10245,#10246,#10247,#10248,#10249,#10250,#10251,#10252,#10253,#10254,
#10255),.UNSPECIFIED.,.F.,.F.,(4,3,3,3,3,3,3,3,3,4),(-0.152712908768378,
-0.128963682254188,-0.116304008925778,-0.092453135123643,-0.0875380734791113,
-0.0797852913889514,-0.0558105568475602,-0.0400274901149945,-0.0159798645019078,
0.),.UNSPECIFIED.);
#187=B_SPLINE_CURVE_WITH_KNOTS('',3,(#10257,#10258,#10259,#10260,#10261,
#10262),.UNSPECIFIED.,.F.,.F.,(4,2,4),(-0.607607610897069,-0.304406883675693,
-0.000702187548907163),.UNSPECIFIED.);
#188=B_SPLINE_CURVE_WITH_KNOTS('',3,(#10268,#10269,#10270,#10271),
 .UNSPECIFIED.,.F.,.F.,(4,4),(0.0130288733793136,0.619909717328002),
 .UNSPECIFIED.);
#189=B_SPLINE_CURVE_WITH_KNOTS('',3,(#10275,#10276,#10277,#10278),
 .UNSPECIFIED.,.F.,.F.,(4,4),(-0.619909717328002,-0.0130288733793137),
 .UNSPECIFIED.);
#190=B_SPLINE_CURVE_WITH_KNOTS('',3,(#10281,#10282,#10283,#10284,#10285,
#10286,#10287),.UNSPECIFIED.,.F.,.F.,(4,3,4),(7.87274532319472,10.4298004347969,
10.9780233963721),.UNSPECIFIED.);
#191=B_SPLINE_CURVE_WITH_KNOTS('',3,(#10288,#10289,#10290,#10291,#10292,
#10293,#10294),.UNSPECIFIED.,.F.,.F.,(4,3,4),(0.511752108249611,2.84807862798167,
3.61537599721027),.UNSPECIFIED.);
#192=B_SPLINE_CURVE_WITH_KNOTS('',3,(#10297,#10298,#10299,#10300,#10301,
#10302,#10303),.UNSPECIFIED.,.F.,.F.,(4,3,4),(3.81523717927831,5.72635044542746,
7.61820606472736),.UNSPECIFIED.);
#193=B_SPLINE_CURVE_WITH_KNOTS('',3,(#10306,#10307,#10308,#10309),
 .UNSPECIFIED.,.F.,.F.,(4,4),(7.8195516254834,10.6519234170402),
 .UNSPECIFIED.);
#194=B_SPLINE_CURVE_WITH_KNOTS('',3,(#10313,#10314,#10315,#10316),
 .UNSPECIFIED.,.F.,.F.,(4,4),(10.8550709503701,11.4839159448819),
 .UNSPECIFIED.);
#195=B_SPLINE_CURVE_WITH_KNOTS('',3,(#10317,#10318,#10319,#10320,#10321,
#10322,#10323,#10324,#10325,#10326,#10327,#10328,#10329,#10330,#10331,#10332,
#10333,#10334,#10335,#10336,#10337,#10338,#10339,#10340,#10341,#10342,#10343,
#10344),.UNSPECIFIED.,.F.,.F.,(4,3,3,3,3,3,3,3,3,4),(0.,0.023800266251022,
0.0390470051780055,0.062864594207143,0.0692752090304052,0.0780196763370091,
0.101808338076191,0.108235461704482,0.131970324379069,0.138468980573541),
 .UNSPECIFIED.);
#196=B_SPLINE_CURVE_WITH_KNOTS('',3,(#10348,#10349,#10350,#10351,#10352,
#10353,#10354,#10355,#10356,#10357,#10358,#10359,#10360,#10361,#10362,#10363,
#10364,#10365,#10366,#10367,#10368,#10369,#10370,#10371,#10372,#10373,#10374,
#10375,#10376,#10377,#10378),.UNSPECIFIED.,.F.,.F.,(4,3,3,3,3,3,3,3,3,3,
4),(0.,0.0536158767337707,0.107707970980176,0.117140678528723,0.171373940961503,
0.178118425384842,0.234058785038521,0.2884659822146,0.324708667187819,0.378759781373182,
0.415412568437851),.UNSPECIFIED.);
#197=B_SPLINE_CURVE_WITH_KNOTS('',3,(#10380,#10381,#10382,#10383),
 .UNSPECIFIED.,.F.,.F.,(4,4),(0.0202983903462145,0.977465912237707),
 .UNSPECIFIED.);
#198=B_SPLINE_CURVE_WITH_KNOTS('',3,(#10385,#10386,#10387,#10388,#10389,
#10390,#10391,#10392,#10393,#10394,#10395,#10396,#10397,#10398,#10399,#10400,
#10401,#10402,#10403,#10404,#10405,#10406,#10407,#10408,#10409,#10410,#10411,
#10412,#10413,#10414,#10415),.UNSPECIFIED.,.F.,.F.,(4,3,3,3,3,3,3,3,3,3,
4),(0.,0.053547205187505,0.107728964525782,0.117299670245694,0.171524652009909,
0.189842726242433,0.234296321023441,0.288773621215207,0.338477936388461,
0.392564001789548,0.442713223041249),.UNSPECIFIED.);
#199=B_SPLINE_CURVE_WITH_KNOTS('',3,(#10419,#10420,#10421,#10422,#10423,
#10424,#10425,#10426,#10427,#10428,#10429,#10430,#10431,#10432,#10433,#10434,
#10435,#10436,#10437,#10438,#10439,#10440,#10441,#10442,#10443,#10444,#10445,
#10446,#10447,#10448,#10449),.UNSPECIFIED.,.F.,.F.,(4,3,3,3,3,3,3,3,3,3,
4),(0.,0.0535312152416108,0.107707123412492,0.117215931328448,0.171445047002381,
0.189808362521926,0.234165405003858,0.288639615809812,0.338404447092272,
0.392504428396833,0.442708851597914),.UNSPECIFIED.);
#200=B_SPLINE_CURVE_WITH_KNOTS('',3,(#10451,#10452,#10453,#10454),
 .UNSPECIFIED.,.F.,.F.,(4,4),(0.0225340877622936,0.979701609653785),
 .UNSPECIFIED.);
#201=B_SPLINE_CURVE_WITH_KNOTS('',3,(#10456,#10457,#10458,#10459,#10460,
#10461,#10462,#10463,#10464,#10465,#10466,#10467,#10468,#10469,#10470,#10471,
#10472,#10473,#10474,#10475,#10476,#10477,#10478,#10479,#10480,#10481,#10482,
#10483,#10484,#10485,#10486),.UNSPECIFIED.,.F.,.F.,(4,3,3,3,3,3,3,3,3,3,
4),(0.,0.0536458552170769,0.107744721567334,0.117297895480617,0.171522683869793,
0.178177673384308,0.23429412186666,0.288702228477357,0.324838815929715,
0.378862861687027,0.415420074045746),.UNSPECIFIED.);
#202=B_SPLINE_CURVE_WITH_KNOTS('',3,(#10489,#10490,#10491,#10492,#10493,
#10494,#10495,#10496,#10497,#10498,#10499,#10500,#10501,#10502,#10503,#10504,
#10505,#10506,#10507,#10508,#10509,#10510,#10511,#10512,#10513,#10514,#10515,
#10516),.UNSPECIFIED.,.F.,.F.,(4,3,3,3,3,3,3,3,3,4),(0.,0.0238098951475563,
0.0390995920428052,0.0629117710415135,0.0692953339558167,0.0780985718814299,
0.101889748471939,0.108278926258091,0.132003149848588,0.138471484390145),
 .UNSPECIFIED.);
#203=B_SPLINE_CURVE_WITH_KNOTS('',3,(#10518,#10519,#10520,#10521),
 .UNSPECIFIED.,.F.,.F.,(4,4),(2.05597917304345E-5,0.629200412657851),
 .UNSPECIFIED.);
#204=B_SPLINE_CURVE_WITH_KNOTS('',3,(#10524,#10525,#10526,#10527),
 .UNSPECIFIED.,.F.,.F.,(4,4),(0.832456091119126,3.6663340257767),
 .UNSPECIFIED.);
#205=B_SPLINE_CURVE_WITH_KNOTS('',3,(#10530,#10531,#10532,#10533,#10534,
#10535,#10536),.UNSPECIFIED.,.F.,.F.,(4,3,4),(3.86778652923942,5.76006783397632,
7.67277763234621),.UNSPECIFIED.);
#206=B_SPLINE_CURVE_WITH_KNOTS('',3,(#10540,#10541,#10542,#10543),
 .UNSPECIFIED.,.F.,.F.,(4,4),(11.1789026308149,11.490024089745),
 .UNSPECIFIED.);
#207=B_SPLINE_CURVE_WITH_KNOTS('',3,(#10545,#10546,#10547,#10548,#10549,
#10550,#10551,#10552,#10553,#10554,#10555,#10556,#10557,#10558,#10559,#10560,
#10561,#10562,#10563,#10564,#10565,#10566,#10567,#10568,#10569),
 .UNSPECIFIED.,.F.,.F.,(4,3,3,3,3,3,3,3,4),(0.,0.0238050540413609,0.0390723036702896,
0.0632692088215501,0.0780555758269344,0.101951849921082,0.112801451778717,
0.136536488207902,0.147568670144067),.UNSPECIFIED.);
#208=B_SPLINE_CURVE_WITH_KNOTS('',3,(#10573,#10574,#10575,#10576,#10577,
#10578,#10579,#10580,#10581,#10582,#10583,#10584,#10585,#10586,#10587,#10588,
#10589,#10590,#10591,#10592,#10593,#10594,#10595,#10596,#10597),
 .UNSPECIFIED.,.F.,.F.,(4,3,3,3,3,3,3,3,4),(0.,0.0238098889950854,0.0391003179068551,
0.0632803937136523,0.0780994777107358,0.101997157448698,0.112825962756833,
0.136555142506291,0.147570127973408),.UNSPECIFIED.);
#209=B_SPLINE_CURVE_WITH_KNOTS('',3,(#10599,#10600,#10601,#10602),
 .UNSPECIFIED.,.F.,.F.,(4,4),(2.41556456535008E-5,0.310979882704647),
 .UNSPECIFIED.);
#210=B_SPLINE_CURVE_WITH_KNOTS('',3,(#10614,#10615,#10616,#10617,#10618,
#10619),.UNSPECIFIED.,.F.,.F.,(4,2,4),(-0.606744425054929,-0.30369469419025,
-0.000104868936493974),.UNSPECIFIED.);
#211=B_SPLINE_CURVE_WITH_KNOTS('',3,(#10621,#10622,#10623,#10624,#10625,
#10626),.UNSPECIFIED.,.F.,.F.,(4,2,4),(-0.60732337425873,-0.303694522808999,
-0.000683832228057069),.UNSPECIFIED.);
#212=B_SPLINE_CURVE_WITH_KNOTS('',3,(#10628,#10629,#10630,#10631,#10632,
#10633,#10634,#10635,#10636,#10637,#10638,#10639,#10640,#10641,#10642,#10643,
#10644,#10645,#10646,#10647,#10648,#10649,#10650,#10651,#10652,#10653,#10654,
#10655),.UNSPECIFIED.,.F.,.F.,(4,3,3,3,3,3,3,3,3,4),(-0.152213081758773,
-0.128388856548194,-0.115047734630008,-0.0910986092737131,-0.0779187269986961,
-0.0651565114518209,-0.0413397067626705,-0.0389038209724845,-0.0151251319644201,
0.),.UNSPECIFIED.);
#213=B_SPLINE_CURVE_WITH_KNOTS('',3,(#10658,#10659,#10660,#10661,#10662,
#10663,#10664,#10665,#10666,#10667,#10668,#10669,#10670,#10671,#10672,#10673,
#10674,#10675,#10676,#10677,#10678,#10679,#10680,#10681,#10682,#10683,#10684,
#10685),.UNSPECIFIED.,.F.,.F.,(4,3,3,3,3,3,3,3,3,4),(-0.152240567100014,
-0.128476012965191,-0.115503482174674,-0.0917060839439778,-0.0870941983819305,
-0.0787260045726768,-0.0547958477503903,-0.0394103419198022,-0.0155561788900784,
0.),.UNSPECIFIED.);
#214=B_SPLINE_CURVE_WITH_KNOTS('',3,(#10702,#10703,#10704,#10705),
 .UNSPECIFIED.,.F.,.F.,(4,4),(-3.85438678954986,-0.750511952447855),
 .UNSPECIFIED.);
#215=B_SPLINE_CURVE_WITH_KNOTS('',3,(#10723,#10724,#10725,#10726),
 .UNSPECIFIED.,.F.,.F.,(4,4),(-0.54981857912664,-0.270878787657975),
 .UNSPECIFIED.);
#216=B_SPLINE_CURVE_WITH_KNOTS('',3,(#10727,#10728,#10729,#10730),
 .UNSPECIFIED.,.F.,.F.,(4,4),(-0.618764321025346,-0.0114172178585034),
 .UNSPECIFIED.);
#217=B_SPLINE_CURVE_WITH_KNOTS('',3,(#10751,#10752,#10753,#10754),
 .UNSPECIFIED.,.F.,.F.,(4,4),(0.74118252158834,3.84969085360113),
 .UNSPECIFIED.);
#218=B_SPLINE_CURVE_WITH_KNOTS('',3,(#10776,#10777,#10778,#10779),
 .UNSPECIFIED.,.F.,.F.,(4,4),(0.270878787657975,0.540284107299618),
 .UNSPECIFIED.);
#219=B_SPLINE_CURVE_WITH_KNOTS('',3,(#10782,#10783,#10784,#10785),
 .UNSPECIFIED.,.F.,.F.,(4,4),(8.04418106222393,11.1526893942367),
 .UNSPECIFIED.);
#220=B_SPLINE_CURVE_WITH_KNOTS('',3,(#10788,#10789,#10790,#10791),
 .UNSPECIFIED.,.F.,.F.,(4,4),(11.3535878085254,11.6229931281671),
 .UNSPECIFIED.);
#221=B_SPLINE_CURVE_WITH_KNOTS('',3,(#10813,#10814,#10815,#10816),
 .UNSPECIFIED.,.F.,.F.,(4,4),(-11.1433599633772,-8.03948512627517),
 .UNSPECIFIED.);
#222=B_SPLINE_CURVE_WITH_KNOTS('',3,(#10850,#10851,#10852,#10853),
 .UNSPECIFIED.,.F.,.F.,(4,4),(0.0114172178585033,0.618764321025346),
 .UNSPECIFIED.);
#223=B_SPLINE_CURVE_WITH_KNOTS('',3,(#10854,#10855,#10856,#10857),
 .UNSPECIFIED.,.F.,.F.,(4,4),(-11.6229931281671,-11.3440533366984),
 .UNSPECIFIED.);
#224=B_SPLINE_CURVE_WITH_KNOTS('',3,(#10860,#10861,#10862,#10863,#10864,
#10865),.UNSPECIFIED.,.F.,.F.,(4,2,4),(-0.606286853269513,-0.303735636734938,
-0.000134370544016882),.UNSPECIFIED.);
#225=B_SPLINE_CURVE_WITH_KNOTS('',3,(#10867,#10868,#10869,#10870,#10871,
#10872,#10873,#10874,#10875,#10876,#10877,#10878,#10879,#10880,#10881,#10882,
#10883,#10884,#10885,#10886,#10887,#10888,#10889,#10890,#10891,#10892,#10893,
#10894),.UNSPECIFIED.,.F.,.F.,(4,3,3,3,3,3,3,3,3,4),(-0.152301724526365,
-0.128559761662057,-0.115189905045126,-0.0912708316251271,-0.0780855696141105,
-0.0652713768517459,-0.0414777101816728,-0.0390314967756457,-0.015242903619151,
0.),.UNSPECIFIED.);
#226=B_SPLINE_CURVE_WITH_KNOTS('',3,(#10898,#10899,#10900,#10901,#10902,
#10903,#10904,#10905,#10906,#10907,#10908,#10909,#10910,#10911,#10912,#10913,
#10914,#10915,#10916,#10917,#10918,#10919,#10920,#10921,#10922,#10923,#10924,
#10925),.UNSPECIFIED.,.F.,.F.,(4,3,3,3,3,3,3,3,3,4),(-0.1523073815286,-0.1285346644938,
-0.115283264026726,-0.0915123087981378,-0.0870533687950649,-0.0782507800682277,
-0.0543447803816484,-0.0391350231834537,-0.0153679399182895,0.),
 .UNSPECIFIED.);
#227=B_SPLINE_CURVE_WITH_KNOTS('',3,(#10926,#10927,#10928,#10929,#10930,
#10931),.UNSPECIFIED.,.F.,.F.,(4,2,4),(-0.607338074051965,-0.303735662161239,
-0.00118557149519966),.UNSPECIFIED.);
#228=B_SPLINE_CURVE_WITH_KNOTS('',3,(#10948,#10949,#10950,#10951),
 .UNSPECIFIED.,.F.,.F.,(4,4),(-7.8460657686783,-4.05419673417835),
 .UNSPECIFIED.);
#229=B_SPLINE_CURVE_WITH_KNOTS('',3,(#10972,#10973,#10974,#10975),
 .UNSPECIFIED.,.F.,.F.,(4,4),(4.04989375377528,7.85140214144331),
 .UNSPECIFIED.);
#230=B_SPLINE_CURVE_WITH_KNOTS('',3,(#10977,#10978,#10979,#10980),
 .UNSPECIFIED.,.F.,.F.,(4,4),(4.0424697743818,7.84397816204974),
 .UNSPECIFIED.);
#231=B_SPLINE_CURVE_WITH_KNOTS('',3,(#11001,#11002,#11003,#11004),
 .UNSPECIFIED.,.F.,.F.,(4,4),(-7.83967518164668,-4.0478061471468),
 .UNSPECIFIED.);
#232=B_SPLINE_CURVE_WITH_KNOTS('',3,(#11023,#11024,#11025,#11026,#11027,
#11028),.UNSPECIFIED.,.F.,.F.,(4,2,4),(-0.606398914035431,-0.303967092551845,
-0.000200694235479137),.UNSPECIFIED.);
#233=B_SPLINE_CURVE_WITH_KNOTS('',3,(#11030,#11031,#11032,#11033,#11034,
#11035,#11036,#11037,#11038,#11039,#11040,#11041,#11042,#11043,#11044,#11045,
#11046,#11047,#11048,#11049,#11050,#11051,#11052,#11053,#11054,#11055,#11056,
#11057),.UNSPECIFIED.,.F.,.F.,(4,3,3,3,3,3,3,3,3,4),(-0.15233244131821,
-0.128569871170003,-0.115181988990177,-0.0912564475476021,-0.0780459432968613,
-0.0652662335163151,-0.0414674738832469,-0.0390013640446512,-0.0152139229936509,
0.),.UNSPECIFIED.);
#234=B_SPLINE_CURVE_WITH_KNOTS('',3,(#11061,#11062,#11063,#11064,#11065,
#11066,#11067,#11068,#11069,#11070,#11071,#11072,#11073,#11074,#11075,#11076,
#11077,#11078,#11079,#11080,#11081,#11082,#11083,#11084,#11085,#11086,#11087,
#11088),.UNSPECIFIED.,.F.,.F.,(4,3,3,3,3,3,3,3,3,4),(-0.152343297533924,
-0.128571042154168,-0.115361098257144,-0.0915841820623439,-0.0870924557961151,
-0.0783628838319633,-0.0544516462338148,-0.0392000432438046,-0.0154115240971992,
0.),.UNSPECIFIED.);
#235=B_SPLINE_CURVE_WITH_KNOTS('',3,(#11089,#11090,#11091,#11092,#11093,
#11094),.UNSPECIFIED.,.F.,.F.,(4,2,4),(-0.607734321217702,-0.303967174049374,
-0.00153607519677973),.UNSPECIFIED.);
#236=B_SPLINE_CURVE_WITH_KNOTS('',3,(#11111,#11112,#11113,#11114),
 .UNSPECIFIED.,.F.,.F.,(4,4),(-10.8531956503852,-8.0457708503995),
 .UNSPECIFIED.);
#237=B_SPLINE_CURVE_WITH_KNOTS('',3,(#11135,#11136,#11137,#11138),
 .UNSPECIFIED.,.F.,.F.,(4,4),(8.05172912332209,10.8690635835914),
 .UNSPECIFIED.);
#238=B_SPLINE_CURVE_WITH_KNOTS('',3,(#11140,#11141,#11142,#11143),
 .UNSPECIFIED.,.F.,.F.,(4,4),(1.02480833223363,3.84214279250303),
 .UNSPECIFIED.);
#239=B_SPLINE_CURVE_WITH_KNOTS('',3,(#11164,#11165,#11166,#11167),
 .UNSPECIFIED.,.F.,.F.,(4,4),(-3.8481010654256,-1.04067626543981),
 .UNSPECIFIED.);
#240=B_SPLINE_CURVE_WITH_KNOTS('',3,(#11186,#11187,#11188,#11189,#11190,
#11191),.UNSPECIFIED.,.F.,.F.,(4,2,4),(-0.608301643694891,-0.304416323412316,
-0.0013178649037765),.UNSPECIFIED.);
#241=B_SPLINE_CURVE_WITH_KNOTS('',3,(#11193,#11194,#11195,#11196,#11197,
#11198,#11199,#11200,#11201,#11202,#11203,#11204,#11205,#11206,#11207,#11208,
#11209,#11210,#11211,#11212,#11213,#11214,#11215,#11216,#11217,#11218,#11219,
#11220),.UNSPECIFIED.,.F.,.F.,(4,3,3,3,3,3,3,3,3,4),(-0.152679905805259,
-0.128657903528546,-0.116982385578132,-0.0929502017086943,-0.0774957796939621,
-0.0651567901405441,-0.0412920018136918,-0.0385809476656748,-0.0148252868187304,
0.),.UNSPECIFIED.);
#242=B_SPLINE_CURVE_WITH_KNOTS('',3,(#11224,#11225,#11226,#11227,#11228,
#11229,#11230,#11231,#11232,#11233,#11234,#11235,#11236,#11237,#11238,#11239,
#11240,#11241,#11242,#11243,#11244,#11245,#11246,#11247,#11248,#11249,#11250,
#11251),.UNSPECIFIED.,.F.,.F.,(4,3,3,3,3,3,3,3,3,4),(-0.152762160496458,
-0.129013039804674,-0.116418683706179,-0.0925605502531877,-0.0875939536119484,
-0.0799546107253736,-0.055976748465099,-0.0401263304884301,-0.0160466564276224,
0.),.UNSPECIFIED.);
#243=B_SPLINE_CURVE_WITH_KNOTS('',3,(#11252,#11253,#11254,#11255,#11256,
#11257),.UNSPECIFIED.,.F.,.F.,(4,2,4),(-0.607519387555057,-0.304417308507995,
-0.000535579674449116),.UNSPECIFIED.);
#244=B_SPLINE_CURVE_WITH_KNOTS('',3,(#11275,#11276,#11277,#11278),
 .UNSPECIFIED.,.F.,.F.,(4,4),(0.012184405392802,0.619909717328002),
 .UNSPECIFIED.);
#245=B_SPLINE_CURVE_WITH_KNOTS('',3,(#11279,#11280,#11281,#11282),
 .UNSPECIFIED.,.F.,.F.,(4,4),(-11.6488871259622,-11.0550486447215),
 .UNSPECIFIED.);
#246=B_SPLINE_CURVE_WITH_KNOTS('',3,(#11305,#11306,#11307,#11308),
 .UNSPECIFIED.,.F.,.F.,(4,4),(11.0717103908866,11.6488871259622),
 .UNSPECIFIED.);
#247=B_SPLINE_CURVE_WITH_KNOTS('',3,(#11312,#11313,#11314,#11315),
 .UNSPECIFIED.,.F.,.F.,(4,4),(0.244984789862841,0.822161524938444),
 .UNSPECIFIED.);
#248=B_SPLINE_CURVE_WITH_KNOTS('',3,(#11333,#11334,#11335,#11336),
 .UNSPECIFIED.,.F.,.F.,(4,4),(-0.838823271103535,-0.244984789862841),
 .UNSPECIFIED.);
#249=B_SPLINE_CURVE_WITH_KNOTS('',3,(#11337,#11338,#11339,#11340),
 .UNSPECIFIED.,.F.,.F.,(4,4),(-0.619909717328002,-0.0121844053928019),
 .UNSPECIFIED.);
#250=B_SPLINE_CURVE_WITH_KNOTS('',3,(#11420,#11421,#11422,#11423),
 .UNSPECIFIED.,.F.,.F.,(4,4),(0.011877999214525,0.618764321025346),
 .UNSPECIFIED.);
#251=B_SPLINE_CURVE_WITH_KNOTS('',3,(#11444,#11445,#11446,#11447),
 .UNSPECIFIED.,.F.,.F.,(4,4),(-0.618764321025346,-0.0118779992145249),
 .UNSPECIFIED.);
#252=B_SPLINE_CURVE_WITH_KNOTS('',3,(#11533,#11534,#11535,#11536),
 .UNSPECIFIED.,.F.,.F.,(4,4),(-1.34441069388203E-17,0.619909717328002),
 .UNSPECIFIED.);
#253=B_SPLINE_CURVE_WITH_KNOTS('',3,(#11537,#11538,#11539,#11540),
 .UNSPECIFIED.,.F.,.F.,(4,4),(-0.619909717328002,-0.00253319281730041),
 .UNSPECIFIED.);
#254=B_SPLINE_CURVE_WITH_KNOTS('',3,(#11581,#11582,#11583,#11584,#11585,
#11586),.UNSPECIFIED.,.F.,.F.,(4,1,1,4),(-11.6488871259622,-8.39802760073243,
-5.14716807550265,-0.270878787657975),.UNSPECIFIED.);
#255=B_SPLINE_CURVE_WITH_KNOTS('',3,(#11587,#11588,#11589,#11590,#11591,
#11592),.UNSPECIFIED.,.F.,.F.,(4,1,1,4),(0.270878787657975,5.14716807550265,
8.39802760073243,11.6488871259622),.UNSPECIFIED.);
#256=B_SPLINE_CURVE_WITH_KNOTS('',3,(#11613,#11614,#11615,#11616),
 .UNSPECIFIED.,.F.,.F.,(4,4),(0.0013822243147816,0.618764321025346),
 .UNSPECIFIED.);
#257=B_SPLINE_CURVE_WITH_KNOTS('',3,(#11617,#11618,#11619,#11620),
 .UNSPECIFIED.,.F.,.F.,(4,4),(-0.618764321025346,8.06646416329215E-17),
 .UNSPECIFIED.);
#258=B_SPLINE_CURVE_WITH_KNOTS('',3,(#11641,#11642,#11643,#11644),
 .UNSPECIFIED.,.F.,.F.,(4,4),(-9.36750677027476E-17,0.618764321025346),
 .UNSPECIFIED.);
#259=B_SPLINE_CURVE_WITH_KNOTS('',3,(#11645,#11646,#11647,#11648),
 .UNSPECIFIED.,.F.,.F.,(4,4),(-0.618764321025346,-0.00138222431478148),
 .UNSPECIFIED.);
#260=B_SPLINE_CURVE_WITH_KNOTS('',3,(#11674,#11675,#11676,#11677,#11678),
 .UNSPECIFIED.,.F.,.F.,(4,1,4),(-11.6229931281671,-5.12127407770751,-0.244984789862841),
 .UNSPECIFIED.);
#261=B_SPLINE_CURVE_WITH_KNOTS('',3,(#11679,#11680,#11681,#11682,#11683),
 .UNSPECIFIED.,.F.,.F.,(4,1,4),(0.244984789862841,5.12127407770751,11.6229931281671),
 .UNSPECIFIED.);
#262=B_SPLINE_CURVE_WITH_KNOTS('',3,(#11704,#11705,#11706,#11707),
 .UNSPECIFIED.,.F.,.F.,(4,4),(0.00253319281730024,0.619909717328002),
 .UNSPECIFIED.);
#263=B_SPLINE_CURVE_WITH_KNOTS('',3,(#11708,#11709,#11710,#11711),
 .UNSPECIFIED.,.F.,.F.,(4,4),(-0.619909717328002,-2.51534904016637E-17),
 .UNSPECIFIED.);
#264=B_SPLINE_CURVE_WITH_KNOTS('',3,(#11953,#11954,#11955,#11956,#11957,
#11958),.UNSPECIFIED.,.F.,.F.,(4,2,4),(-0.607240122656937,-0.303691721894415,
-0.000634514333697656),.UNSPECIFIED.);
#265=B_SPLINE_CURVE_WITH_KNOTS('',3,(#11960,#11961,#11962,#11963,#11964,
#11965,#11966,#11967,#11968,#11969,#11970,#11971,#11972,#11973,#11974,#11975,
#11976,#11977,#11978,#11979,#11980,#11981,#11982,#11983,#11984,#11985,#11986,
#11987),.UNSPECIFIED.,.F.,.F.,(4,3,3,3,3,3,3,3,3,4),(-0.152223584381152,
-0.128403685910756,-0.115058138924018,-0.0911105876986024,-0.0779275105489685,
-0.0651650823668383,-0.0413494676927402,-0.0389105926748606,-0.0151313403168948,
0.),.UNSPECIFIED.);
#266=B_SPLINE_CURVE_WITH_KNOTS('',3,(#11991,#11992,#11993,#11994,#11995,
#11996,#11997,#11998,#11999,#12000,#12001,#12002,#12003,#12004,#12005,#12006,
#12007,#12008,#12009,#12010,#12011,#12012,#12013,#12014,#12015,#12016,#12017,
#12018),.UNSPECIFIED.,.F.,.F.,(4,3,3,3,3,3,3,3,3,4),(-0.152249917238265,
-0.128484865669312,-0.115494642307313,-0.0916985948709881,-0.0870953287403626,
-0.0787006597758974,-0.0547717013112817,-0.0393956522318865,-0.0155460991587222,
0.),.UNSPECIFIED.);
#267=B_SPLINE_CURVE_WITH_KNOTS('',3,(#12019,#12020,#12021,#12022,#12023,
#12024),.UNSPECIFIED.,.F.,.F.,(4,2,4),(-0.606785315485727,-0.30369188913634,
-0.000179692314978108),.UNSPECIFIED.);
#268=B_SPLINE_CURVE_WITH_KNOTS('',3,(#12029,#12030,#12031,#12032,#12033,
#12034),.UNSPECIFIED.,.F.,.F.,(4,2,4),(-0.606332812995025,-0.303737653350621,
-0.000161665236032726),.UNSPECIFIED.);
#269=B_SPLINE_CURVE_WITH_KNOTS('',3,(#12036,#12037,#12038,#12039,#12040,
#12041,#12042,#12043,#12044,#12045,#12046,#12047,#12048,#12049,#12050,#12051,
#12052,#12053,#12054,#12055,#12056,#12057,#12058,#12059,#12060,#12061,#12062,
#12063),.UNSPECIFIED.,.F.,.F.,(4,3,3,3,3,3,3,3,3,4),(-0.152301160038588,
-0.128555435257278,-0.115184785848022,-0.0912639339035621,-0.0780773216554274,
-0.065267350293706,-0.0414723266145325,-0.0390252168402571,-0.0152374671294611,
0.),.UNSPECIFIED.);
#270=B_SPLINE_CURVE_WITH_KNOTS('',3,(#12067,#12068,#12069,#12070,#12071,
#12072,#12073,#12074,#12075,#12076,#12077,#12078,#12079,#12080,#12081,#12082,
#12083,#12084,#12085,#12086,#12087,#12088,#12089,#12090,#12091,#12092,#12093,
#12094),.UNSPECIFIED.,.F.,.F.,(4,3,3,3,3,3,3,3,3,4),(-0.152307894271445,
-0.128535938708366,-0.115295945509717,-0.0915234088298753,-0.0870575315710991,
-0.0782740392368046,-0.0543664511067997,-0.0391484926712317,-0.0153774171089249,
0.),.UNSPECIFIED.);
#271=B_SPLINE_CURVE_WITH_KNOTS('',3,(#12096,#12097,#12098,#12099,#12100,
#12101),.UNSPECIFIED.,.F.,.F.,(4,2,4),(-0.607315067615316,-0.303737782617996,
-0.00114390098251854),.UNSPECIFIED.);
#272=B_SPLINE_CURVE_WITH_KNOTS('',3,(#12107,#12108,#12109,#12110,#12111,
#12112),.UNSPECIFIED.,.F.,.F.,(4,2,4),(-0.606335618682527,-0.303964064424246,
-0.000163142902895597),.UNSPECIFIED.);
#273=B_SPLINE_CURVE_WITH_KNOTS('',3,(#12114,#12115,#12116,#12117,#12118,
#12119,#12120,#12121,#12122,#12123,#12124,#12125,#12126,#12127,#12128,#12129,
#12130,#12131,#12132,#12133,#12134,#12135,#12136,#12137,#12138,#12139,#12140,
#12141),.UNSPECIFIED.,.F.,.F.,(4,3,3,3,3,3,3,3,3,4),(-0.152324888062519,
-0.128571266282871,-0.115187819092559,-0.0912644922975459,-0.0780623053857969,
-0.0652705430018984,-0.0414736125245103,-0.0390138150290758,-0.015226502089553,
0.),.UNSPECIFIED.);
#274=B_SPLINE_CURVE_WITH_KNOTS('',3,(#12145,#12146,#12147,#12148,#12149,
#12150,#12151,#12152,#12153,#12154,#12155,#12156,#12157,#12158,#12159,#12160,
#12161,#12162,#12163,#12164,#12165,#12166,#12167,#12168,#12169,#12170,#12171,
#12172),.UNSPECIFIED.,.F.,.F.,(4,3,3,3,3,3,3,3,3,4),(-0.152333600285603,
-0.128561769460285,-0.115331525958272,-0.0915566852459163,-0.0870792380259527,
-0.0783165909319309,-0.0544069520497563,-0.0391732033593778,-0.0153939862842036,
0.),.UNSPECIFIED.);
#275=B_SPLINE_CURVE_WITH_KNOTS('',3,(#12174,#12175,#12176,#12177,#12178,
#12179),.UNSPECIFIED.,.F.,.F.,(4,2,4),(-0.607765665607205,-0.303964210965506,
-0.00159316434717749),.UNSPECIFIED.);
#276=B_SPLINE_CURVE_WITH_KNOTS('',3,(#12185,#12186,#12187,#12188,#12189,
#12190),.UNSPECIFIED.,.F.,.F.,(4,2,4),(-0.608113833554089,-0.304405910662044,
-0.00120843896277512),.UNSPECIFIED.);
#277=B_SPLINE_CURVE_WITH_KNOTS('',3,(#12192,#12193,#12194,#12195,#12196,
#12197,#12198,#12199,#12200,#12201,#12202,#12203,#12204,#12205,#12206,#12207,
#12208,#12209,#12210,#12211,#12212,#12213,#12214,#12215,#12216,#12217,#12218,
#12219),.UNSPECIFIED.,.F.,.F.,(4,3,3,3,3,3,3,3,3,4),(-0.152638346832965,
-0.128647829044501,-0.117000727359648,-0.0929750760194364,-0.0775532335837778,
-0.065166230851578,-0.0413072760700971,-0.0386249916896363,-0.0148681833632798,
0.),.UNSPECIFIED.);
#278=B_SPLINE_CURVE_WITH_KNOTS('',3,(#12223,#12224,#12225,#12226,#12227,
#12228,#12229,#12230,#12231,#12232,#12233,#12234,#12235,#12236,#12237,#12238,
#12239,#12240,#12241,#12242,#12243,#12244,#12245,#12246,#12247,#12248,#12249,
#12250),.UNSPECIFIED.,.F.,.F.,(4,3,3,3,3,3,3,3,3,4),(-0.152712908768378,
-0.128963682254188,-0.116304008925778,-0.092453135123643,-0.0875380734791113,
-0.0797852913889514,-0.0558105568475602,-0.0400274901149945,-0.0159798645019078,
0.),.UNSPECIFIED.);
#279=B_SPLINE_CURVE_WITH_KNOTS('',3,(#12252,#12253,#12254,#12255,#12256,
#12257),.UNSPECIFIED.,.F.,.F.,(4,2,4),(-0.607607610897069,-0.304406883675693,
-0.000702187548907163),.UNSPECIFIED.);
#280=B_SPLINE_CURVE_WITH_KNOTS('',3,(#12263,#12264,#12265,#12266),
 .UNSPECIFIED.,.F.,.F.,(4,4),(0.0130288733793136,0.619909717328002),
 .UNSPECIFIED.);
#281=B_SPLINE_CURVE_WITH_KNOTS('',3,(#12270,#12271,#12272,#12273),
 .UNSPECIFIED.,.F.,.F.,(4,4),(-0.619909717328002,-0.0130288733793137),
 .UNSPECIFIED.);
#282=B_SPLINE_CURVE_WITH_KNOTS('',3,(#12276,#12277,#12278,#12279,#12280,
#12281,#12282),.UNSPECIFIED.,.F.,.F.,(4,3,4),(7.87274532319472,10.4298004347969,
10.9780233963721),.UNSPECIFIED.);
#283=B_SPLINE_CURVE_WITH_KNOTS('',3,(#12283,#12284,#12285,#12286,#12287,
#12288,#12289),.UNSPECIFIED.,.F.,.F.,(4,3,4),(0.511752108249611,2.84807862798167,
3.61537599721027),.UNSPECIFIED.);
#284=B_SPLINE_CURVE_WITH_KNOTS('',3,(#12292,#12293,#12294,#12295,#12296,
#12297,#12298),.UNSPECIFIED.,.F.,.F.,(4,3,4),(3.81523717927831,5.72635044542746,
7.61820606472736),.UNSPECIFIED.);
#285=B_SPLINE_CURVE_WITH_KNOTS('',3,(#12301,#12302,#12303,#12304),
 .UNSPECIFIED.,.F.,.F.,(4,4),(7.8195516254834,10.6519234170402),
 .UNSPECIFIED.);
#286=B_SPLINE_CURVE_WITH_KNOTS('',3,(#12308,#12309,#12310,#12311),
 .UNSPECIFIED.,.F.,.F.,(4,4),(10.8550709503701,11.4839159448819),
 .UNSPECIFIED.);
#287=B_SPLINE_CURVE_WITH_KNOTS('',3,(#12312,#12313,#12314,#12315,#12316,
#12317,#12318,#12319,#12320,#12321,#12322,#12323,#12324,#12325,#12326,#12327,
#12328,#12329,#12330,#12331,#12332,#12333,#12334,#12335,#12336,#12337,#12338,
#12339),.UNSPECIFIED.,.F.,.F.,(4,3,3,3,3,3,3,3,3,4),(0.,0.023800266251022,
0.0390470051780055,0.062864594207143,0.0692752090304052,0.0780196763370091,
0.101808338076191,0.108235461704482,0.131970324379069,0.138468980573541),
 .UNSPECIFIED.);
#288=B_SPLINE_CURVE_WITH_KNOTS('',3,(#12343,#12344,#12345,#12346,#12347,
#12348,#12349,#12350,#12351,#12352,#12353,#12354,#12355,#12356,#12357,#12358,
#12359,#12360,#12361,#12362,#12363,#12364,#12365,#12366,#12367,#12368,#12369,
#12370,#12371,#12372,#12373),.UNSPECIFIED.,.F.,.F.,(4,3,3,3,3,3,3,3,3,3,
4),(0.,0.0536158767337707,0.107707970980176,0.117140678528723,0.171373940961503,
0.178118425384842,0.234058785038521,0.2884659822146,0.324708667187819,0.378759781373182,
0.415412568437851),.UNSPECIFIED.);
#289=B_SPLINE_CURVE_WITH_KNOTS('',3,(#12375,#12376,#12377,#12378),
 .UNSPECIFIED.,.F.,.F.,(4,4),(0.0202983903462145,0.977465912237707),
 .UNSPECIFIED.);
#290=B_SPLINE_CURVE_WITH_KNOTS('',3,(#12380,#12381,#12382,#12383,#12384,
#12385,#12386,#12387,#12388,#12389,#12390,#12391,#12392,#12393,#12394,#12395,
#12396,#12397,#12398,#12399,#12400,#12401,#12402,#12403,#12404,#12405,#12406,
#12407,#12408,#12409,#12410),.UNSPECIFIED.,.F.,.F.,(4,3,3,3,3,3,3,3,3,3,
4),(0.,0.053547205187505,0.107728964525782,0.117299670245694,0.171524652009909,
0.189842726242433,0.234296321023441,0.288773621215207,0.338477936388461,
0.392564001789548,0.442713223041249),.UNSPECIFIED.);
#291=B_SPLINE_CURVE_WITH_KNOTS('',3,(#12414,#12415,#12416,#12417,#12418,
#12419,#12420,#12421,#12422,#12423,#12424,#12425,#12426,#12427,#12428,#12429,
#12430,#12431,#12432,#12433,#12434,#12435,#12436,#12437,#12438,#12439,#12440,
#12441,#12442,#12443,#12444),.UNSPECIFIED.,.F.,.F.,(4,3,3,3,3,3,3,3,3,3,
4),(0.,0.0535312152416108,0.107707123412492,0.117215931328448,0.171445047002381,
0.189808362521926,0.234165405003858,0.288639615809812,0.338404447092272,
0.392504428396833,0.442708851597914),.UNSPECIFIED.);
#292=B_SPLINE_CURVE_WITH_KNOTS('',3,(#12446,#12447,#12448,#12449),
 .UNSPECIFIED.,.F.,.F.,(4,4),(0.0225340877622936,0.979701609653785),
 .UNSPECIFIED.);
#293=B_SPLINE_CURVE_WITH_KNOTS('',3,(#12451,#12452,#12453,#12454,#12455,
#12456,#12457,#12458,#12459,#12460,#12461,#12462,#12463,#12464,#12465,#12466,
#12467,#12468,#12469,#12470,#12471,#12472,#12473,#12474,#12475,#12476,#12477,
#12478,#12479,#12480,#12481),.UNSPECIFIED.,.F.,.F.,(4,3,3,3,3,3,3,3,3,3,
4),(0.,0.0536458552170769,0.107744721567334,0.117297895480617,0.171522683869793,
0.178177673384308,0.23429412186666,0.288702228477357,0.324838815929715,
0.378862861687027,0.415420074045746),.UNSPECIFIED.);
#294=B_SPLINE_CURVE_WITH_KNOTS('',3,(#12484,#12485,#12486,#12487,#12488,
#12489,#12490,#12491,#12492,#12493,#12494,#12495,#12496,#12497,#12498,#12499,
#12500,#12501,#12502,#12503,#12504,#12505,#12506,#12507,#12508,#12509,#12510,
#12511),.UNSPECIFIED.,.F.,.F.,(4,3,3,3,3,3,3,3,3,4),(0.,0.0238098951475563,
0.0390995920428052,0.0629117710415135,0.0692953339558167,0.0780985718814299,
0.101889748471939,0.108278926258091,0.132003149848588,0.138471484390145),
 .UNSPECIFIED.);
#295=B_SPLINE_CURVE_WITH_KNOTS('',3,(#12513,#12514,#12515,#12516),
 .UNSPECIFIED.,.F.,.F.,(4,4),(2.05597917304345E-5,0.629200412657851),
 .UNSPECIFIED.);
#296=B_SPLINE_CURVE_WITH_KNOTS('',3,(#12519,#12520,#12521,#12522),
 .UNSPECIFIED.,.F.,.F.,(4,4),(0.832456091119126,3.6663340257767),
 .UNSPECIFIED.);
#297=B_SPLINE_CURVE_WITH_KNOTS('',3,(#12525,#12526,#12527,#12528,#12529,
#12530,#12531),.UNSPECIFIED.,.F.,.F.,(4,3,4),(3.86778652923942,5.76006783397632,
7.67277763234621),.UNSPECIFIED.);
#298=B_SPLINE_CURVE_WITH_KNOTS('',3,(#12535,#12536,#12537,#12538),
 .UNSPECIFIED.,.F.,.F.,(4,4),(11.1789026308149,11.490024089745),
 .UNSPECIFIED.);
#299=B_SPLINE_CURVE_WITH_KNOTS('',3,(#12540,#12541,#12542,#12543,#12544,
#12545,#12546,#12547,#12548,#12549,#12550,#12551,#12552,#12553,#12554,#12555,
#12556,#12557,#12558,#12559,#12560,#12561,#12562,#12563,#12564),
 .UNSPECIFIED.,.F.,.F.,(4,3,3,3,3,3,3,3,4),(0.,0.0238050540413609,0.0390723036702896,
0.0632692088215501,0.0780555758269344,0.101951849921082,0.112801451778717,
0.136536488207902,0.147568670144067),.UNSPECIFIED.);
#300=B_SPLINE_CURVE_WITH_KNOTS('',3,(#12568,#12569,#12570,#12571,#12572,
#12573,#12574,#12575,#12576,#12577,#12578,#12579,#12580,#12581,#12582,#12583,
#12584,#12585,#12586,#12587,#12588,#12589,#12590,#12591,#12592),
 .UNSPECIFIED.,.F.,.F.,(4,3,3,3,3,3,3,3,4),(0.,0.0238098889950854,0.0391003179068551,
0.0632803937136523,0.0780994777107358,0.101997157448698,0.112825962756833,
0.136555142506291,0.147570127973408),.UNSPECIFIED.);
#301=B_SPLINE_CURVE_WITH_KNOTS('',3,(#12594,#12595,#12596,#12597),
 .UNSPECIFIED.,.F.,.F.,(4,4),(2.41556456535008E-5,0.310979882704647),
 .UNSPECIFIED.);
#302=B_SPLINE_CURVE_WITH_KNOTS('',3,(#12609,#12610,#12611,#12612,#12613,
#12614),.UNSPECIFIED.,.F.,.F.,(4,2,4),(-0.606744425054929,-0.30369469419025,
-0.000104868936493974),.UNSPECIFIED.);
#303=B_SPLINE_CURVE_WITH_KNOTS('',3,(#12616,#12617,#12618,#12619,#12620,
#12621),.UNSPECIFIED.,.F.,.F.,(4,2,4),(-0.60732337425873,-0.303694522808999,
-0.000683832228057069),.UNSPECIFIED.);
#304=B_SPLINE_CURVE_WITH_KNOTS('',3,(#12623,#12624,#12625,#12626,#12627,
#12628,#12629,#12630,#12631,#12632,#12633,#12634,#12635,#12636,#12637,#12638,
#12639,#12640,#12641,#12642,#12643,#12644,#12645,#12646,#12647,#12648,#12649,
#12650),.UNSPECIFIED.,.F.,.F.,(4,3,3,3,3,3,3,3,3,4),(-0.152213081758773,
-0.128388856548194,-0.115047734630008,-0.0910986092737131,-0.0779187269986961,
-0.0651565114518209,-0.0413397067626705,-0.0389038209724845,-0.0151251319644201,
0.),.UNSPECIFIED.);
#305=B_SPLINE_CURVE_WITH_KNOTS('',3,(#12653,#12654,#12655,#12656,#12657,
#12658,#12659,#12660,#12661,#12662,#12663,#12664,#12665,#12666,#12667,#12668,
#12669,#12670,#12671,#12672,#12673,#12674,#12675,#12676,#12677,#12678,#12679,
#12680),.UNSPECIFIED.,.F.,.F.,(4,3,3,3,3,3,3,3,3,4),(-0.152240567100014,
-0.128476012965191,-0.115503482174674,-0.0917060839439778,-0.0870941983819305,
-0.0787260045726768,-0.0547958477503903,-0.0394103419198022,-0.0155561788900784,
0.),.UNSPECIFIED.);
#306=B_SPLINE_CURVE_WITH_KNOTS('',3,(#12697,#12698,#12699,#12700),
 .UNSPECIFIED.,.F.,.F.,(4,4),(-3.85438678954986,-0.750511952447855),
 .UNSPECIFIED.);
#307=B_SPLINE_CURVE_WITH_KNOTS('',3,(#12718,#12719,#12720,#12721),
 .UNSPECIFIED.,.F.,.F.,(4,4),(-0.54981857912664,-0.270878787657975),
 .UNSPECIFIED.);
#308=B_SPLINE_CURVE_WITH_KNOTS('',3,(#12722,#12723,#12724,#12725),
 .UNSPECIFIED.,.F.,.F.,(4,4),(-0.618764321025346,-0.0114172178585034),
 .UNSPECIFIED.);
#309=B_SPLINE_CURVE_WITH_KNOTS('',3,(#12746,#12747,#12748,#12749),
 .UNSPECIFIED.,.F.,.F.,(4,4),(0.74118252158834,3.84969085360113),
 .UNSPECIFIED.);
#310=B_SPLINE_CURVE_WITH_KNOTS('',3,(#12771,#12772,#12773,#12774),
 .UNSPECIFIED.,.F.,.F.,(4,4),(0.270878787657975,0.540284107299618),
 .UNSPECIFIED.);
#311=B_SPLINE_CURVE_WITH_KNOTS('',3,(#12777,#12778,#12779,#12780),
 .UNSPECIFIED.,.F.,.F.,(4,4),(8.04418106222393,11.1526893942367),
 .UNSPECIFIED.);
#312=B_SPLINE_CURVE_WITH_KNOTS('',3,(#12783,#12784,#12785,#12786),
 .UNSPECIFIED.,.F.,.F.,(4,4),(11.3535878085254,11.6229931281671),
 .UNSPECIFIED.);
#313=B_SPLINE_CURVE_WITH_KNOTS('',3,(#12808,#12809,#12810,#12811),
 .UNSPECIFIED.,.F.,.F.,(4,4),(-11.1433599633772,-8.03948512627517),
 .UNSPECIFIED.);
#314=B_SPLINE_CURVE_WITH_KNOTS('',3,(#12845,#12846,#12847,#12848),
 .UNSPECIFIED.,.F.,.F.,(4,4),(0.0114172178585033,0.618764321025346),
 .UNSPECIFIED.);
#315=B_SPLINE_CURVE_WITH_KNOTS('',3,(#12849,#12850,#12851,#12852),
 .UNSPECIFIED.,.F.,.F.,(4,4),(-11.6229931281671,-11.3440533366984),
 .UNSPECIFIED.);
#316=B_SPLINE_CURVE_WITH_KNOTS('',3,(#12855,#12856,#12857,#12858,#12859,
#12860),.UNSPECIFIED.,.F.,.F.,(4,2,4),(-0.606286853269513,-0.303735636734938,
-0.000134370544016882),.UNSPECIFIED.);
#317=B_SPLINE_CURVE_WITH_KNOTS('',3,(#12862,#12863,#12864,#12865,#12866,
#12867,#12868,#12869,#12870,#12871,#12872,#12873,#12874,#12875,#12876,#12877,
#12878,#12879,#12880,#12881,#12882,#12883,#12884,#12885,#12886,#12887,#12888,
#12889),.UNSPECIFIED.,.F.,.F.,(4,3,3,3,3,3,3,3,3,4),(-0.152301724526365,
-0.128559761662057,-0.115189905045126,-0.0912708316251271,-0.0780855696141105,
-0.0652713768517459,-0.0414777101816728,-0.0390314967756457,-0.015242903619151,
0.),.UNSPECIFIED.);
#318=B_SPLINE_CURVE_WITH_KNOTS('',3,(#12893,#12894,#12895,#12896,#12897,
#12898,#12899,#12900,#12901,#12902,#12903,#12904,#12905,#12906,#12907,#12908,
#12909,#12910,#12911,#12912,#12913,#12914,#12915,#12916,#12917,#12918,#12919,
#12920),.UNSPECIFIED.,.F.,.F.,(4,3,3,3,3,3,3,3,3,4),(-0.1523073815286,-0.1285346644938,
-0.115283264026726,-0.0915123087981378,-0.0870533687950649,-0.0782507800682277,
-0.0543447803816484,-0.0391350231834537,-0.0153679399182895,0.),
 .UNSPECIFIED.);
#319=B_SPLINE_CURVE_WITH_KNOTS('',3,(#12921,#12922,#12923,#12924,#12925,
#12926),.UNSPECIFIED.,.F.,.F.,(4,2,4),(-0.607338074051965,-0.303735662161239,
-0.00118557149519966),.UNSPECIFIED.);
#320=B_SPLINE_CURVE_WITH_KNOTS('',3,(#12943,#12944,#12945,#12946),
 .UNSPECIFIED.,.F.,.F.,(4,4),(-7.8460657686783,-4.05419673417835),
 .UNSPECIFIED.);
#321=B_SPLINE_CURVE_WITH_KNOTS('',3,(#12967,#12968,#12969,#12970),
 .UNSPECIFIED.,.F.,.F.,(4,4),(4.04989375377528,7.85140214144331),
 .UNSPECIFIED.);
#322=B_SPLINE_CURVE_WITH_KNOTS('',3,(#12972,#12973,#12974,#12975),
 .UNSPECIFIED.,.F.,.F.,(4,4),(4.0424697743818,7.84397816204974),
 .UNSPECIFIED.);
#323=B_SPLINE_CURVE_WITH_KNOTS('',3,(#12996,#12997,#12998,#12999),
 .UNSPECIFIED.,.F.,.F.,(4,4),(-7.83967518164668,-4.0478061471468),
 .UNSPECIFIED.);
#324=B_SPLINE_CURVE_WITH_KNOTS('',3,(#13018,#13019,#13020,#13021,#13022,
#13023),.UNSPECIFIED.,.F.,.F.,(4,2,4),(-0.606398914035431,-0.303967092551845,
-0.000200694235479137),.UNSPECIFIED.);
#325=B_SPLINE_CURVE_WITH_KNOTS('',3,(#13025,#13026,#13027,#13028,#13029,
#13030,#13031,#13032,#13033,#13034,#13035,#13036,#13037,#13038,#13039,#13040,
#13041,#13042,#13043,#13044,#13045,#13046,#13047,#13048,#13049,#13050,#13051,
#13052),.UNSPECIFIED.,.F.,.F.,(4,3,3,3,3,3,3,3,3,4),(-0.15233244131821,
-0.128569871170003,-0.115181988990177,-0.0912564475476021,-0.0780459432968613,
-0.0652662335163151,-0.0414674738832469,-0.0390013640446512,-0.0152139229936509,
0.),.UNSPECIFIED.);
#326=B_SPLINE_CURVE_WITH_KNOTS('',3,(#13056,#13057,#13058,#13059,#13060,
#13061,#13062,#13063,#13064,#13065,#13066,#13067,#13068,#13069,#13070,#13071,
#13072,#13073,#13074,#13075,#13076,#13077,#13078,#13079,#13080,#13081,#13082,
#13083),.UNSPECIFIED.,.F.,.F.,(4,3,3,3,3,3,3,3,3,4),(-0.152343297533924,
-0.128571042154168,-0.115361098257144,-0.0915841820623439,-0.0870924557961151,
-0.0783628838319633,-0.0544516462338148,-0.0392000432438046,-0.0154115240971992,
0.),.UNSPECIFIED.);
#327=B_SPLINE_CURVE_WITH_KNOTS('',3,(#13084,#13085,#13086,#13087,#13088,
#13089),.UNSPECIFIED.,.F.,.F.,(4,2,4),(-0.607734321217702,-0.303967174049374,
-0.00153607519677973),.UNSPECIFIED.);
#328=B_SPLINE_CURVE_WITH_KNOTS('',3,(#13106,#13107,#13108,#13109),
 .UNSPECIFIED.,.F.,.F.,(4,4),(-10.8531956503852,-8.0457708503995),
 .UNSPECIFIED.);
#329=B_SPLINE_CURVE_WITH_KNOTS('',3,(#13130,#13131,#13132,#13133),
 .UNSPECIFIED.,.F.,.F.,(4,4),(8.05172912332209,10.8690635835914),
 .UNSPECIFIED.);
#330=B_SPLINE_CURVE_WITH_KNOTS('',3,(#13135,#13136,#13137,#13138),
 .UNSPECIFIED.,.F.,.F.,(4,4),(1.02480833223363,3.84214279250303),
 .UNSPECIFIED.);
#331=B_SPLINE_CURVE_WITH_KNOTS('',3,(#13159,#13160,#13161,#13162),
 .UNSPECIFIED.,.F.,.F.,(4,4),(-3.8481010654256,-1.04067626543981),
 .UNSPECIFIED.);
#332=B_SPLINE_CURVE_WITH_KNOTS('',3,(#13181,#13182,#13183,#13184,#13185,
#13186),.UNSPECIFIED.,.F.,.F.,(4,2,4),(-0.608301643694891,-0.304416323412316,
-0.0013178649037765),.UNSPECIFIED.);
#333=B_SPLINE_CURVE_WITH_KNOTS('',3,(#13188,#13189,#13190,#13191,#13192,
#13193,#13194,#13195,#13196,#13197,#13198,#13199,#13200,#13201,#13202,#13203,
#13204,#13205,#13206,#13207,#13208,#13209,#13210,#13211,#13212,#13213,#13214,
#13215),.UNSPECIFIED.,.F.,.F.,(4,3,3,3,3,3,3,3,3,4),(-0.152679905805259,
-0.128657903528546,-0.116982385578132,-0.0929502017086943,-0.0774957796939621,
-0.0651567901405441,-0.0412920018136918,-0.0385809476656748,-0.0148252868187304,
0.),.UNSPECIFIED.);
#334=B_SPLINE_CURVE_WITH_KNOTS('',3,(#13219,#13220,#13221,#13222,#13223,
#13224,#13225,#13226,#13227,#13228,#13229,#13230,#13231,#13232,#13233,#13234,
#13235,#13236,#13237,#13238,#13239,#13240,#13241,#13242,#13243,#13244,#13245,
#13246),.UNSPECIFIED.,.F.,.F.,(4,3,3,3,3,3,3,3,3,4),(-0.152762160496458,
-0.129013039804674,-0.116418683706179,-0.0925605502531877,-0.0875939536119484,
-0.0799546107253736,-0.055976748465099,-0.0401263304884301,-0.0160466564276224,
0.),.UNSPECIFIED.);
#335=B_SPLINE_CURVE_WITH_KNOTS('',3,(#13247,#13248,#13249,#13250,#13251,
#13252),.UNSPECIFIED.,.F.,.F.,(4,2,4),(-0.607519387555057,-0.304417308507995,
-0.000535579674449116),.UNSPECIFIED.);
#336=B_SPLINE_CURVE_WITH_KNOTS('',3,(#13270,#13271,#13272,#13273),
 .UNSPECIFIED.,.F.,.F.,(4,4),(0.012184405392802,0.619909717328002),
 .UNSPECIFIED.);
#337=B_SPLINE_CURVE_WITH_KNOTS('',3,(#13274,#13275,#13276,#13277),
 .UNSPECIFIED.,.F.,.F.,(4,4),(-11.6488871259622,-11.0550486447215),
 .UNSPECIFIED.);
#338=B_SPLINE_CURVE_WITH_KNOTS('',3,(#13300,#13301,#13302,#13303),
 .UNSPECIFIED.,.F.,.F.,(4,4),(11.0717103908866,11.6488871259622),
 .UNSPECIFIED.);
#339=B_SPLINE_CURVE_WITH_KNOTS('',3,(#13307,#13308,#13309,#13310),
 .UNSPECIFIED.,.F.,.F.,(4,4),(0.244984789862841,0.822161524938444),
 .UNSPECIFIED.);
#340=B_SPLINE_CURVE_WITH_KNOTS('',3,(#13328,#13329,#13330,#13331),
 .UNSPECIFIED.,.F.,.F.,(4,4),(-0.838823271103535,-0.244984789862841),
 .UNSPECIFIED.);
#341=B_SPLINE_CURVE_WITH_KNOTS('',3,(#13332,#13333,#13334,#13335),
 .UNSPECIFIED.,.F.,.F.,(4,4),(-0.619909717328002,-0.0121844053928019),
 .UNSPECIFIED.);
#342=B_SPLINE_CURVE_WITH_KNOTS('',3,(#13415,#13416,#13417,#13418),
 .UNSPECIFIED.,.F.,.F.,(4,4),(0.011877999214525,0.618764321025346),
 .UNSPECIFIED.);
#343=B_SPLINE_CURVE_WITH_KNOTS('',3,(#13439,#13440,#13441,#13442),
 .UNSPECIFIED.,.F.,.F.,(4,4),(-0.618764321025346,-0.0118779992145249),
 .UNSPECIFIED.);
#344=B_SPLINE_CURVE_WITH_KNOTS('',3,(#13528,#13529,#13530,#13531),
 .UNSPECIFIED.,.F.,.F.,(4,4),(-1.34441069388203E-17,0.619909717328002),
 .UNSPECIFIED.);
#345=B_SPLINE_CURVE_WITH_KNOTS('',3,(#13532,#13533,#13534,#13535),
 .UNSPECIFIED.,.F.,.F.,(4,4),(-0.619909717328002,-0.00253319281730041),
 .UNSPECIFIED.);
#346=B_SPLINE_CURVE_WITH_KNOTS('',3,(#13576,#13577,#13578,#13579,#13580,
#13581),.UNSPECIFIED.,.F.,.F.,(4,1,1,4),(-11.6488871259622,-8.39802760073243,
-5.14716807550265,-0.270878787657975),.UNSPECIFIED.);
#347=B_SPLINE_CURVE_WITH_KNOTS('',3,(#13582,#13583,#13584,#13585,#13586,
#13587),.UNSPECIFIED.,.F.,.F.,(4,1,1,4),(0.270878787657975,5.14716807550265,
8.39802760073243,11.6488871259622),.UNSPECIFIED.);
#348=B_SPLINE_CURVE_WITH_KNOTS('',3,(#13608,#13609,#13610,#13611),
 .UNSPECIFIED.,.F.,.F.,(4,4),(0.0013822243147816,0.618764321025346),
 .UNSPECIFIED.);
#349=B_SPLINE_CURVE_WITH_KNOTS('',3,(#13612,#13613,#13614,#13615),
 .UNSPECIFIED.,.F.,.F.,(4,4),(-0.618764321025346,8.06646416329215E-17),
 .UNSPECIFIED.);
#350=B_SPLINE_CURVE_WITH_KNOTS('',3,(#13636,#13637,#13638,#13639),
 .UNSPECIFIED.,.F.,.F.,(4,4),(-9.36750677027476E-17,0.618764321025346),
 .UNSPECIFIED.);
#351=B_SPLINE_CURVE_WITH_KNOTS('',3,(#13640,#13641,#13642,#13643),
 .UNSPECIFIED.,.F.,.F.,(4,4),(-0.618764321025346,-0.00138222431478148),
 .UNSPECIFIED.);
#352=B_SPLINE_CURVE_WITH_KNOTS('',3,(#13669,#13670,#13671,#13672,#13673),
 .UNSPECIFIED.,.F.,.F.,(4,1,4),(-11.6229931281671,-5.12127407770751,-0.244984789862841),
 .UNSPECIFIED.);
#353=B_SPLINE_CURVE_WITH_KNOTS('',3,(#13674,#13675,#13676,#13677,#13678),
 .UNSPECIFIED.,.F.,.F.,(4,1,4),(0.244984789862841,5.12127407770751,11.6229931281671),
 .UNSPECIFIED.);
#354=B_SPLINE_CURVE_WITH_KNOTS('',3,(#13699,#13700,#13701,#13702),
 .UNSPECIFIED.,.F.,.F.,(4,4),(0.00253319281730024,0.619909717328002),
 .UNSPECIFIED.);
#355=B_SPLINE_CURVE_WITH_KNOTS('',3,(#13703,#13704,#13705,#13706),
 .UNSPECIFIED.,.F.,.F.,(4,4),(-0.619909717328002,-2.51534904016637E-17),
 .UNSPECIFIED.);
#356=B_SPLINE_CURVE_WITH_KNOTS('',3,(#13840,#13841,#13842,#13843,#13844),
 .UNSPECIFIED.,.F.,.F.,(4,1,4),(-0.102486762950766,-0.0439228984074713,
0.),.UNSPECIFIED.);
#357=B_SPLINE_CURVE_WITH_KNOTS('',3,(#13847,#13848,#13849,#13850,#13851),
 .UNSPECIFIED.,.F.,.F.,(4,1,4),(0.,0.0439228984074713,0.102486762950766),
 .UNSPECIFIED.);
#358=B_SPLINE_CURVE_WITH_KNOTS('',3,(#13886,#13887,#13888,#13889,#13890),
 .UNSPECIFIED.,.F.,.F.,(4,1,4),(-0.102486763046448,-0.0439228984484775,
0.),.UNSPECIFIED.);
#359=B_SPLINE_CURVE_WITH_KNOTS('',3,(#13891,#13892,#13893,#13894,#13895),
 .UNSPECIFIED.,.F.,.F.,(4,1,4),(0.,0.0439228984484775,0.102486763046448),
 .UNSPECIFIED.);
#360=B_SPLINE_CURVE_WITH_KNOTS('',3,(#13929,#13930,#13931,#13932,#13933,
#13934),.UNSPECIFIED.,.F.,.F.,(4,1,1,4),(-11.061861191744,-7.9013294226743,
-4.74079765360458,0.),.UNSPECIFIED.);
#361=B_SPLINE_CURVE_WITH_KNOTS('',3,(#13935,#13936,#13937,#13938,#13939,
#13940),.UNSPECIFIED.,.F.,.F.,(4,1,1,4),(0.,4.74079765360458,7.9013294226743,
11.061861191744),.UNSPECIFIED.);
#362=B_SPLINE_CURVE_WITH_KNOTS('',3,(#13969,#13970,#13971,#13972,#13973),
 .UNSPECIFIED.,.F.,.F.,(4,1,4),(-0.0955241394393374,-0.0409389169025732,
0.),.UNSPECIFIED.);
#363=B_SPLINE_CURVE_WITH_KNOTS('',3,(#13974,#13975,#13976,#13977,#13978),
 .UNSPECIFIED.,.F.,.F.,(4,1,4),(0.,0.0409389169025732,0.0955241394393374),
 .UNSPECIFIED.);
#364=B_SPLINE_CURVE_WITH_KNOTS('',3,(#14013,#14014,#14015,#14016,#14017),
 .UNSPECIFIED.,.F.,.F.,(4,1,4),(-0.0955241391394202,-0.054585222365383,
-2.31010434703409E-17),.UNSPECIFIED.);
#365=B_SPLINE_CURVE_WITH_KNOTS('',3,(#14018,#14019,#14020,#14021,#14022),
 .UNSPECIFIED.,.F.,.F.,(4,1,4),(2.31010434703409E-17,0.054585222365383,
0.0955241391394202),.UNSPECIFIED.);
#366=B_SPLINE_CURVE_WITH_KNOTS('',3,(#14053,#14054,#14055,#14056,#14057,
#14058),.UNSPECIFIED.,.F.,.F.,(4,1,1,4),(-11.0618420179497,-6.32105258168553,
-3.16052629084276,-1.48308270761676E-15),.UNSPECIFIED.);
#367=B_SPLINE_CURVE_WITH_KNOTS('',3,(#14059,#14060,#14061,#14062,#14063,
#14064),.UNSPECIFIED.,.F.,.F.,(4,1,1,4),(1.48308270761676E-15,3.16052629084276,
6.32105258168553,11.0618420179497),.UNSPECIFIED.);
#368=B_SPLINE_CURVE_WITH_KNOTS('',3,(#14067,#14068,#14069,#14070),
 .UNSPECIFIED.,.F.,.F.,(4,4),(0.00139191041679171,0.12591792480537),
 .UNSPECIFIED.);
#369=B_SPLINE_CURVE_WITH_KNOTS('',3,(#14073,#14074,#14075,#14076),
 .UNSPECIFIED.,.F.,.F.,(4,4),(-0.12591792480537,-0.00139191041679165),
 .UNSPECIFIED.);
#370=B_SPLINE_CURVE_WITH_KNOTS('',3,(#14098,#14099,#14100,#14101),
 .UNSPECIFIED.,.F.,.F.,(4,4),(-0.125267757839186,2.34187669256869E-17),
 .UNSPECIFIED.);
#371=B_SPLINE_CURVE_WITH_KNOTS('',3,(#14102,#14103,#14104,#14105,#14106,
#14107,#14108,#14109,#14110,#14111,#14112,#14113,#14114,#14115,#14116,#14117,
#14118,#14119,#14120,#14121,#14122,#14123,#14124,#14125,#14126),
 .UNSPECIFIED.,.F.,.F.,(4,3,3,3,3,3,3,3,4),(0.,0.0322618866145428,0.0585630993998112,
0.0880157356071287,0.11701919887454,0.14936655709923,0.161132799378038,
0.193259076308563,0.205272292311979),.UNSPECIFIED.);
#372=B_SPLINE_CURVE_WITH_KNOTS('',3,(#14144,#14145,#14146,#14147),
 .UNSPECIFIED.,.F.,.F.,(4,4),(-1.85615411929518E-16,0.12492953807382),
 .UNSPECIFIED.);
#373=B_SPLINE_CURVE_WITH_KNOTS('',3,(#14148,#14149,#14150,#14151),
 .UNSPECIFIED.,.F.,.F.,(4,4),(0.0105624938889701,0.988135278219398),
 .UNSPECIFIED.);
#374=B_SPLINE_CURVE_WITH_KNOTS('',3,(#14173,#14174,#14175,#14176),
 .UNSPECIFIED.,.F.,.F.,(4,4),(-0.125282751535517,-0.000756099764976127),
 .UNSPECIFIED.);
#375=B_SPLINE_CURVE_WITH_KNOTS('',3,(#14177,#14178,#14179,#14180,#14181,
#14182,#14183,#14184,#14185,#14186,#14187,#14188,#14189,#14190,#14191,#14192,
#14193,#14194,#14195,#14196,#14197,#14198,#14199,#14200,#14201,#14202,#14203,
#14204),.UNSPECIFIED.,.F.,.F.,(4,3,3,3,3,3,3,3,3,4),(0.,0.0322721186185131,
0.0586507621648183,0.090893271235385,0.0944607523249211,0.117149429440675,
0.149538018358679,0.168700492523839,0.200858914363656,0.220277485057336),
 .UNSPECIFIED.);
#376=B_SPLINE_CURVE_WITH_KNOTS('',3,(#14208,#14209,#14210,#14211),
 .UNSPECIFIED.,.F.,.F.,(4,4),(0.000756099764976051,0.125282751535516),
 .UNSPECIFIED.);
#377=B_SPLINE_CURVE_WITH_KNOTS('',3,(#14234,#14235,#14236,#14237,#14238,
#14239,#14240,#14241,#14242,#14243,#14244,#14245,#14246,#14247,#14248,#14249,
#14250,#14251,#14252,#14253,#14254,#14255,#14256,#14257,#14258),
 .UNSPECIFIED.,.F.,.F.,(4,3,3,3,3,3,3,3,4),(-1.38777878078145E-17,0.0322740250441291,
0.0586501551213245,0.0880475535304867,0.117148640042868,0.149495851515852,
0.161204029299056,0.193312734374797,0.205276387553207),.UNSPECIFIED.);
#378=B_SPLINE_CURVE_WITH_KNOTS('',3,(#14259,#14260,#14261,#14262),
 .UNSPECIFIED.,.F.,.F.,(4,4),(5.20417042793042E-18,0.125267757839184),
 .UNSPECIFIED.);
#379=B_SPLINE_CURVE_WITH_KNOTS('',3,(#14284,#14285,#14286,#14287),
 .UNSPECIFIED.,.F.,.F.,(4,4),(-0.124929538073804,-1.0547118733939E-15),
 .UNSPECIFIED.);
#380=B_SPLINE_CURVE_WITH_KNOTS('',3,(#14288,#14289,#14290,#14291,#14292,
#14293,#14294,#14295,#14296,#14297,#14298,#14299,#14300,#14301,#14302,#14303,
#14304,#14305,#14306,#14307,#14308,#14309,#14310,#14311,#14312,#14313,#14314,
#14315),.UNSPECIFIED.,.F.,.F.,(4,3,3,3,3,3,3,3,3,4),(0.,0.0322648940196546,
0.0586047006713273,0.0908498906869236,0.0944423330072586,0.117077542275299,
0.149464200283694,0.168660330271145,0.200827593216919,0.220275105166519),
 .UNSPECIFIED.);
#381=B_SPLINE_CURVE_WITH_KNOTS('',3,(#14317,#14318,#14319,#14320),
 .UNSPECIFIED.,.F.,.F.,(4,4),(0.0118647217806024,0.98943750611103),
 .UNSPECIFIED.);
#382=B_SPLINE_CURVE_WITH_KNOTS('',3,(#14343,#14344,#14345,#14346,#14347,
#14348,#14349,#14350,#14351,#14352),.UNSPECIFIED.,.F.,.F.,(4,3,3,4),(-4.09202352044852,
-3.99057144343763,-2.99292858257822,-2.07317267331971),.UNSPECIFIED.);
#383=B_SPLINE_CURVE_WITH_KNOTS('',3,(#14355,#14356,#14357,#14358,#14359,
#14360,#14361),.UNSPECIFIED.,.F.,.F.,(4,3,4),(0.,0.998042281124014,1.12274180646116),
 .UNSPECIFIED.);
#384=B_SPLINE_CURVE_WITH_KNOTS('',3,(#14366,#14367,#14368,#14369,#14370,
#14371,#14372,#14373,#14374,#14375,#14376,#14377,#14378,#14379,#14380,#14381,
#14382,#14383,#14384,#14385,#14386,#14387),.UNSPECIFIED.,.F.,.F.,(4,3,3,
3,3,3,3,4),(-10.3752088276281,-9.97642860859406,-8.97878574773466,-7.98114288687525,
-6.98350002601584,-5.98585716515644,-4.98821430429703,-4.09202352044852),
 .UNSPECIFIED.);
#385=B_SPLINE_CURVE_WITH_KNOTS('',3,(#14388,#14389,#14390,#14391,#14392,
#14393,#14394,#14395,#14396,#14397,#14398,#14399,#14400,#14401,#14402,#14403,
#14404,#14405,#14406,#14407,#14408,#14409),.UNSPECIFIED.,.F.,.F.,(4,3,3,
3,3,3,3,4),(1.12274180646116,1.99608456224804,2.99412684337208,3.99216912449611,
4.99021140562014,5.98825368674417,6.98629596786821,7.40592711364074),
 .UNSPECIFIED.);
#386=B_SPLINE_CURVE_WITH_KNOTS('',3,(#14414,#14415,#14416,#14417,#14418,
#14419,#14420,#14421,#14422,#14423,#14424,#14425,#14426,#14427,#14428,#14429,
#14430,#14431,#14432,#14433,#14434,#14435),.UNSPECIFIED.,.F.,.F.,(4,3,3,
3,3,3,3,4),(-16.6583941348077,-15.9622857737505,-14.9646429128911,-13.9670000520317,
-12.9693571911723,-11.9717143303129,-10.9740714694535,-10.3752088276281),
 .UNSPECIFIED.);
#387=B_SPLINE_CURVE_WITH_KNOTS('',3,(#14436,#14437,#14438,#14439,#14440,
#14441,#14442,#14443,#14444,#14445,#14446,#14447,#14448,#14449,#14450,#14451,
#14452,#14453,#14454,#14455,#14456,#14457),.UNSPECIFIED.,.F.,.F.,(4,3,3,
3,3,3,3,4),(7.40592711364074,7.98433824899223,8.98238053011626,9.98042281124028,
10.9784650923643,11.9765073734883,12.9745496546124,13.6891124208203),
 .UNSPECIFIED.);
#388=B_SPLINE_CURVE_WITH_KNOTS('',3,(#14462,#14463,#14464,#14465,#14466,
#14467,#14468,#14469,#14470,#14471,#14472,#14473,#14474,#14475,#14476,#14477,
#14478,#14479,#14480,#14481,#14482,#14483),.UNSPECIFIED.,.F.,.F.,(4,3,3,
3,3,3,3,4),(-22.9415794419873,-21.9481429389069,-20.9505000780475,-19.9528572171881,
-18.9552143563287,-17.9575714954693,-16.9599286346099,-16.6583941348077),
 .UNSPECIFIED.);
#389=B_SPLINE_CURVE_WITH_KNOTS('',3,(#14484,#14485,#14486,#14487,#14488,
#14489,#14490,#14491,#14492,#14493,#14494,#14495,#14496,#14497,#14498,#14499,
#14500,#14501,#14502,#14503,#14504,#14505,#14506,#14507,#14508),
 .UNSPECIFIED.,.F.,.F.,(4,3,3,3,3,3,3,3,4),(13.6891124208203,13.9725919357364,
14.9706342168604,15.9686764979844,16.9667187791085,17.9647610602325,18.9628033413565,
19.9608456224805,19.9722977279999),.UNSPECIFIED.);
#390=B_SPLINE_CURVE_WITH_KNOTS('',3,(#14513,#14514,#14515,#14516,#14517,
#14518,#14519,#14520,#14521,#14522,#14523,#14524,#14525,#14526,#14527,#14528,
#14529,#14530,#14531,#14532,#14533,#14534),.UNSPECIFIED.,.F.,.F.,(4,3,3,
3,3,3,3,4),(-29.2247647491669,-28.9316429649228,-27.9340001040634,-26.936357243204,
-25.9387143823446,-24.9410715214852,-23.9434286606257,-22.9415794419873),
 .UNSPECIFIED.);
#391=B_SPLINE_CURVE_WITH_KNOTS('',3,(#14535,#14536,#14537,#14538,#14539,
#14540,#14541,#14542,#14543,#14544,#14545,#14546,#14547,#14548,#14549,#14550,
#14551,#14552,#14553,#14554,#14555,#14556),.UNSPECIFIED.,.F.,.F.,(4,3,3,
3,3,3,3,4),(19.9722977279999,20.9588879036046,21.9569301847286,22.9549724658526,
23.9530147469767,24.9510570281007,25.9490993092247,26.2554830351795),
 .UNSPECIFIED.);
#392=B_SPLINE_CURVE_WITH_KNOTS('',3,(#14561,#14562,#14563,#14564,#14565,
#14566,#14567,#14568,#14569,#14570,#14571,#14572,#14573,#14574,#14575,#14576,
#14577,#14578,#14579,#14580,#14581,#14582),.UNSPECIFIED.,.F.,.F.,(4,3,3,
3,3,3,3,4),(-35.5079500563465,-34.9175001300792,-33.9198572692198,-32.9222144083604,
-31.924571547501,-30.9269286866416,-29.9292858257822,-29.2247647491669),
 .UNSPECIFIED.);
#393=B_SPLINE_CURVE_WITH_KNOTS('',3,(#14583,#14584,#14585,#14586,#14587,
#14588,#14589,#14590,#14591,#14592,#14593,#14594,#14595,#14596,#14597,#14598,
#14599,#14600,#14601,#14602,#14603,#14604),.UNSPECIFIED.,.F.,.F.,(4,3,3,
3,3,3,3,4),(26.2554830351795,26.9471415903487,27.9451838714728,28.9432261525968,
29.9412684337208,30.9393107148448,31.9373529959689,32.5386683423591),
 .UNSPECIFIED.);
#394=B_SPLINE_CURVE_WITH_KNOTS('',3,(#14609,#14610,#14611,#14612,#14613,
#14614,#14615,#14616,#14617,#14618,#14619,#14620,#14621,#14622,#14623,#14624,
#14625,#14626,#14627,#14628,#14629,#14630),.UNSPECIFIED.,.F.,.F.,(4,3,3,
3,3,3,3,4),(-41.791135363526,-40.9033572952357,-39.9057144343762,-38.9080715735168,
-37.9104287126574,-36.912785851798,-35.9151429909386,-35.5079500563465),
 .UNSPECIFIED.);
#395=B_SPLINE_CURVE_WITH_KNOTS('',3,(#14631,#14632,#14633,#14634,#14635,
#14636,#14637,#14638,#14639,#14640,#14641,#14642,#14643,#14644,#14645,#14646,
#14647,#14648,#14649,#14650,#14651,#14652),.UNSPECIFIED.,.F.,.F.,(4,3,3,
3,3,3,3,4),(32.5386683423591,32.9353952770929,33.9334375582169,34.931479839341,
35.929522120465,36.927564401589,37.9256066827131,38.8218536495387),
 .UNSPECIFIED.);
#396=B_SPLINE_CURVE_WITH_KNOTS('',3,(#14657,#14658,#14659,#14660,#14661,
#14662,#14663,#14664,#14665,#14666,#14667,#14668,#14669,#14670,#14671,#14672,
#14673,#14674,#14675,#14676,#14677,#14678,#14679,#14680,#14681),
 .UNSPECIFIED.,.F.,.F.,(4,3,3,3,3,3,3,3,4),(-48.0743206707056,-47.8868573212515,
-46.8892144603921,-45.8915715995327,-44.8939287386733,-43.8962858778139,
-42.8986430169545,-41.9010001560951,-41.791135363526),.UNSPECIFIED.);
#397=B_SPLINE_CURVE_WITH_KNOTS('',3,(#14682,#14683,#14684,#14685,#14686,
#14687,#14688,#14689,#14690,#14691,#14692,#14693,#14694,#14695,#14696,#14697,
#14698,#14699,#14700,#14701,#14702,#14703,#14704,#14705,#14706),
 .UNSPECIFIED.,.F.,.F.,(4,3,3,3,3,3,3,3,4),(38.8218536495387,38.9236489638371,
39.9216912449611,40.9197335260851,41.9177758072091,42.9158180883332,43.9138603694572,
44.9119026505812,45.1050389567183),.UNSPECIFIED.);
#398=B_SPLINE_CURVE_WITH_KNOTS('',3,(#14711,#14712,#14713,#14714,#14715,
#14716,#14717,#14718,#14719,#14720,#14721,#14722,#14723,#14724,#14725,#14726,
#14727,#14728,#14729,#14730,#14731,#14732),.UNSPECIFIED.,.F.,.F.,(4,3,3,
3,3,3,3,4),(-54.3575059778852,-53.8727144864079,-52.8750716255485,-51.8774287646891,
-50.8797859038297,-49.8821430429703,-48.8845001821109,-48.0743206707056),
 .UNSPECIFIED.);
#399=B_SPLINE_CURVE_WITH_KNOTS('',3,(#14733,#14734,#14735,#14736,#14737,
#14738,#14739,#14740,#14741,#14742,#14743,#14744,#14745,#14746,#14747,#14748,
#14749,#14750,#14751,#14752,#14753,#14754),.UNSPECIFIED.,.F.,.F.,(4,3,3,
3,3,3,3,4),(45.1050389567183,45.9099449317052,46.9079872128293,47.9060294939533,
48.9040717750773,49.9021140562014,50.9001563373254,51.3882242638979),
 .UNSPECIFIED.);
#400=B_SPLINE_CURVE_WITH_KNOTS('',3,(#14759,#14760,#14761,#14762,#14763,
#14764,#14765,#14766,#14767,#14768,#14769,#14770,#14771,#14772,#14773,#14774,
#14775,#14776,#14777,#14778,#14779,#14780),.UNSPECIFIED.,.F.,.F.,(4,3,3,
3,3,3,3,4),(-60.6406912850648,-59.8585716515644,-58.860928790705,-57.8632859298455,
-56.8656430689861,-55.8680002081267,-54.8703573472673,-54.3575059778852),
 .UNSPECIFIED.);
#401=B_SPLINE_CURVE_WITH_KNOTS('',3,(#14781,#14782,#14783,#14784,#14785,
#14786,#14787,#14788,#14789,#14790,#14791,#14792,#14793,#14794,#14795,#14796,
#14797,#14798,#14799,#14800,#14801,#14802),.UNSPECIFIED.,.F.,.F.,(4,3,3,
3,3,3,3,4),(51.3882242638979,51.8981986184494,52.8962408995734,53.8942831806975,
54.8923254618215,55.8903677429455,56.8884100240695,57.6714095710775),
 .UNSPECIFIED.);
#402=B_SPLINE_CURVE_WITH_KNOTS('',3,(#14807,#14808,#14809,#14810,#14811,
#14812,#14813,#14814,#14815,#14816,#14817,#14818,#14819,#14820,#14821,#14822,
#14823,#14824,#14825,#14826,#14827,#14828,#14829,#14830,#14831),
 .UNSPECIFIED.,.F.,.F.,(4,3,3,3,3,3,3,3,4),(-66.9238765922444,-66.8420716775802,
-65.8444288167208,-64.8467859558614,-63.849143095002,-62.8515002341426,
-61.8538573732832,-60.8562145124238,-60.6406912850648),.UNSPECIFIED.);
#403=B_SPLINE_CURVE_WITH_KNOTS('',3,(#14832,#14833,#14834,#14835,#14836,
#14837,#14838,#14839,#14840,#14841,#14842,#14843,#14844,#14845,#14846,#14847,
#14848,#14849,#14850,#14851,#14852,#14853,#14854,#14855,#14856),
 .UNSPECIFIED.,.F.,.F.,(4,3,3,3,3,3,3,3,4),(57.6714095710775,57.8864523051936,
58.8844945863176,59.8825368674416,60.8805791485657,61.8786214296897,62.8766637108137,
63.8747059919378,63.9545948782571),.UNSPECIFIED.);
#404=B_SPLINE_CURVE_WITH_KNOTS('',3,(#14861,#14862,#14863,#14864,#14865,
#14866,#14867,#14868,#14869,#14870,#14871,#14872,#14873,#14874,#14875,#14876,
#14877,#14878,#14879,#14880,#14881,#14882),.UNSPECIFIED.,.F.,.F.,(4,3,3,
3,3,3,3,4),(-73.207061899424,-72.8279288427366,-71.8302859818773,-70.8326431210178,
-69.8350002601584,-68.837357399299,-67.8397145384396,-66.9238765922444),
 .UNSPECIFIED.);
#405=B_SPLINE_CURVE_WITH_KNOTS('',3,(#14883,#14884,#14885,#14886,#14887,
#14888,#14889,#14890,#14891,#14892,#14893,#14894,#14895,#14896,#14897,#14898,
#14899,#14900,#14901,#14902,#14903,#14904),.UNSPECIFIED.,.F.,.F.,(4,3,3,
3,3,3,3,4),(63.9545948782571,64.8727482730618,65.8707905541858,66.8688328353098,
67.8668751164338,68.8649173975579,69.8629596786819,70.2377801854366),
 .UNSPECIFIED.);
#406=B_SPLINE_CURVE_WITH_KNOTS('',3,(#14909,#14910,#14911,#14912,#14913,
#14914,#14915,#14916,#14917,#14918,#14919,#14920,#14921,#14922,#14923,#14924,
#14925,#14926,#14927,#14928,#14929,#14930),.UNSPECIFIED.,.F.,.F.,(4,3,3,
3,3,3,3,4),(-79.4902472066036,-78.8137860078931,-77.8161431470337,-76.8185002861743,
-75.8208574253149,-74.8232145644555,-73.825571703596,-73.207061899424),
 .UNSPECIFIED.);
#407=B_SPLINE_CURVE_WITH_KNOTS('',3,(#14931,#14932,#14933,#14934,#14935,
#14936,#14937,#14938,#14939,#14940,#14941,#14942,#14943,#14944,#14945,#14946,
#14947,#14948,#14949,#14950,#14951,#14952),.UNSPECIFIED.,.F.,.F.,(4,3,3,
3,3,3,3,4),(70.2377801854366,70.8610019598059,71.85904424093,72.857086522054,
73.855128803178,74.853171084302,75.8512133654261,76.5209654926162),
 .UNSPECIFIED.);
#408=B_SPLINE_CURVE_WITH_KNOTS('',3,(#14957,#14958,#14959,#14960,#14961,
#14962,#14963,#14964,#14965,#14966,#14967,#14968,#14969,#14970,#14971,#14972,
#14973,#14974,#14975,#14976,#14977,#14978),.UNSPECIFIED.,.F.,.F.,(4,3,3,
3,3,3,3,4),(-85.7734325137832,-84.7996431730495,-83.8020003121901,-82.8043574513307,
-81.8067145904713,-80.8090717296119,-79.8114288687525,-79.4902472066036),
 .UNSPECIFIED.);
#409=B_SPLINE_CURVE_WITH_KNOTS('',3,(#14979,#14980,#14981,#14982,#14983,
#14984,#14985,#14986,#14987,#14988,#14989,#14990,#14991,#14992,#14993,#14994,
#14995,#14996,#14997,#14998,#14999,#15000),.UNSPECIFIED.,.F.,.F.,(4,3,3,
3,3,3,3,4),(76.5209654926162,76.8492556465501,77.8472979276741,78.8453402087982,
79.8433824899222,80.8414247710462,81.8394670521702,82.8041507997958),
 .UNSPECIFIED.);
#410=B_SPLINE_CURVE_WITH_KNOTS('',3,(#15005,#15006,#15007,#15008,#15009,
#15010,#15011,#15012,#15013,#15014,#15015,#15016,#15017,#15018,#15019,#15020,
#15021,#15022,#15023,#15024,#15025,#15026,#15027,#15028,#15029),
 .UNSPECIFIED.,.F.,.F.,(4,3,3,3,3,3,3,3,4),(-92.0566178209628,-91.7831431990654,
-90.7855003382059,-89.7878574773465,-88.7902146164871,-87.7925717556277,
-86.7949288947683,-85.7972860339089,-85.7734325137832),.UNSPECIFIED.);
#411=B_SPLINE_CURVE_WITH_KNOTS('',3,(#15030,#15031,#15032,#15033,#15034,
#15035,#15036,#15037,#15038,#15039,#15040,#15041,#15042,#15043,#15044,#15045,
#15046,#15047,#15048,#15049,#15050,#15051,#15052,#15053,#15054),
 .UNSPECIFIED.,.F.,.F.,(4,3,3,3,3,3,3,3,4),(82.8041507997958,82.8375093332942,
83.8355516144183,84.8335938955423,85.8316361766664,86.8296784577904,87.8277207389144,
88.8257630200384,89.0873361069754),.UNSPECIFIED.);
#412=B_SPLINE_CURVE_WITH_KNOTS('',3,(#15059,#15060,#15061,#15062,#15063,
#15064,#15065,#15066,#15067,#15068,#15069,#15070,#15071,#15072,#15073,#15074,
#15075,#15076,#15077,#15078,#15079,#15080),.UNSPECIFIED.,.F.,.F.,(4,3,3,
3,3,3,3,4),(-98.3398031281424,-97.7690003642218,-96.7713575033624,-95.773714642503,
-94.7760717816436,-93.7784289207842,-92.7807860599248,-92.0566178209628),
 .UNSPECIFIED.);
#413=B_SPLINE_CURVE_WITH_KNOTS('',3,(#15081,#15082,#15083,#15084,#15085,
#15086,#15087,#15088,#15089,#15090,#15091,#15092,#15093,#15094,#15095,#15096,
#15097,#15098,#15099,#15100,#15101,#15102),.UNSPECIFIED.,.F.,.F.,(4,3,3,
3,3,3,3,4),(89.0873361069754,89.8238053011624,90.8218475822865,91.8198898634105,
92.8179321445345,93.8159744256585,94.8140167067826,95.370521414155),
 .UNSPECIFIED.);
#414=B_SPLINE_CURVE_WITH_KNOTS('',3,(#15107,#15108,#15109,#15110,#15111,
#15112,#15113,#15114,#15115,#15116,#15117,#15118,#15119,#15120,#15121,#15122,
#15123,#15124,#15125,#15126,#15127,#15128),.UNSPECIFIED.,.F.,.F.,(4,3,3,
3,3,3,3,4),(-104.622988435322,-103.754857529378,-102.757214668519,-101.759571807659,
-100.7619289468,-99.7642860859406,-98.7666432250812,-98.3398031281424),
 .UNSPECIFIED.);
#415=B_SPLINE_CURVE_WITH_KNOTS('',3,(#15129,#15130,#15131,#15132,#15133,
#15134,#15135,#15136,#15137,#15138,#15139,#15140,#15141,#15142,#15143,#15144,
#15145,#15146,#15147,#15148,#15149,#15150),.UNSPECIFIED.,.F.,.F.,(4,3,3,
3,3,3,3,4),(95.370521414155,95.8120589879066,96.8101012690306,97.8081435501546,
98.8061858312787,99.8042281124027,100.802270393527,101.653706721335),
 .UNSPECIFIED.);
#416=B_SPLINE_CURVE_WITH_KNOTS('',3,(#15155,#15156,#15157,#15158,#15159,
#15160,#15161,#15162,#15163,#15164,#15165,#15166,#15167,#15168,#15169,#15170,
#15171,#15172,#15173,#15174,#15175,#15176,#15177,#15178,#15179),
 .UNSPECIFIED.,.F.,.F.,(4,3,3,3,3,3,3,3,4),(-110.906173742502,-110.738357555394,
-109.740714694535,-108.743071833675,-107.745428972816,-106.747786111956,
-105.750143251097,-104.752500390238,-104.622988435322),.UNSPECIFIED.);
#417=B_SPLINE_CURVE_WITH_KNOTS('',3,(#15180,#15181,#15182,#15183,#15184,
#15185,#15186,#15187,#15188,#15189,#15190,#15191,#15192,#15193,#15194,#15195,
#15196,#15197,#15198,#15199,#15200,#15201,#15202,#15203,#15204),
 .UNSPECIFIED.,.F.,.F.,(4,3,3,3,3,3,3,3,4),(101.653706721335,101.800312674651,
102.798354955775,103.796397236899,104.794439518023,105.792481799147,106.790524080271,
107.788566361395,107.936892028514),.UNSPECIFIED.);
#418=B_SPLINE_CURVE_WITH_KNOTS('',3,(#15209,#15210,#15211,#15212,#15213,
#15214,#15215,#15216,#15217,#15218,#15219,#15220,#15221,#15222,#15223,#15224,
#15225,#15226,#15227,#15228,#15229,#15230),.UNSPECIFIED.,.F.,.F.,(4,3,3,
3,3,3,3,4),(-117.189359049681,-116.724214720551,-115.726571859691,-114.728928998832,
-113.731286137972,-112.733643277113,-111.736000416253,-110.906173742502),
 .UNSPECIFIED.);
#419=B_SPLINE_CURVE_WITH_KNOTS('',3,(#15231,#15232,#15233,#15234,#15235,
#15236,#15237,#15238,#15239,#15240,#15241,#15242,#15243,#15244,#15245,#15246,
#15247,#15248,#15249,#15250,#15251,#15252),.UNSPECIFIED.,.F.,.F.,(4,3,3,
3,3,3,3,4),(107.936892028514,108.786608642519,109.784650923643,110.782693204767,
111.780735485891,112.778777767015,113.776820048139,114.220077335694),
 .UNSPECIFIED.);
#420=B_SPLINE_CURVE_WITH_KNOTS('',3,(#15257,#15258,#15259,#15260,#15261,
#15262,#15263,#15264,#15265,#15266,#15267,#15268,#15269,#15270,#15271,#15272,
#15273,#15274,#15275,#15276,#15277,#15278),.UNSPECIFIED.,.F.,.F.,(4,3,3,
3,3,3,3,4),(-123.472544356861,-122.710071885707,-121.712429024848,-120.714786163988,
-119.717143303129,-118.719500442269,-117.72185758141,-117.189359049681),
 .UNSPECIFIED.);
#421=B_SPLINE_CURVE_WITH_KNOTS('',3,(#15279,#15280,#15281,#15282,#15283,
#15284,#15285,#15286,#15287,#15288,#15289,#15290,#15291,#15292,#15293,#15294,
#15295,#15296,#15297,#15298,#15299,#15300),.UNSPECIFIED.,.F.,.F.,(4,3,3,
3,3,3,3,4),(114.220077335694,114.774862329263,115.772904610387,116.770946891511,
117.768989172635,118.767031453759,119.765073734883,120.503262642873),
 .UNSPECIFIED.);
#422=B_SPLINE_CURVE_WITH_KNOTS('',3,(#15305,#15306,#15307,#15308,#15309,
#15310,#15311,#15312,#15313,#15314,#15315,#15316,#15317,#15318,#15319,#15320,
#15321,#15322,#15323,#15324,#15325,#15326,#15327,#15328,#15329),
 .UNSPECIFIED.,.F.,.F.,(4,3,3,3,3,3,3,3,4),(-129.75572966404,-129.693571911723,
-128.695929050863,-127.698286190004,-126.700643329145,-125.703000468285,
-124.705357607426,-123.707714746566,-123.472544356861),.UNSPECIFIED.);
#423=B_SPLINE_CURVE_WITH_KNOTS('',3,(#15330,#15331,#15332,#15333,#15334,
#15335,#15336,#15337,#15338,#15339,#15340,#15341,#15342,#15343,#15344,#15345,
#15346,#15347,#15348,#15349,#15350,#15351,#15352,#15353,#15354),
 .UNSPECIFIED.,.F.,.F.,(4,3,3,3,3,3,3,3,4),(120.503262642873,120.763116016007,
121.761158297131,122.759200578255,123.757242859379,124.755285140503,125.753327421627,
126.751369702751,126.786447950053),.UNSPECIFIED.);
#424=B_SPLINE_CURVE_WITH_KNOTS('',3,(#15359,#15360,#15361,#15362,#15363,
#15364,#15365,#15366,#15367,#15368,#15369,#15370,#15371,#15372,#15373,#15374,
#15375,#15376,#15377,#15378,#15379,#15380),.UNSPECIFIED.,.F.,.F.,(4,3,3,
3,3,3,3,4),(-136.03891497122,-135.679429076879,-134.68178621602,-133.68414335516,
-132.686500494301,-131.688857633442,-130.691214772582,-129.75572966404),
 .UNSPECIFIED.);
#425=B_SPLINE_CURVE_WITH_KNOTS('',3,(#15381,#15382,#15383,#15384,#15385,
#15386,#15387,#15388,#15389,#15390,#15391,#15392,#15393,#15394,#15395,#15396,
#15397,#15398,#15399,#15400,#15401,#15402),.UNSPECIFIED.,.F.,.F.,(4,3,3,
3,3,3,3,4),(126.786447950053,127.749411983875,128.747454265,129.745496546124,
130.743538827248,131.741581108372,132.739623389496,133.069633257233),
 .UNSPECIFIED.);
#426=B_SPLINE_CURVE_WITH_KNOTS('',3,(#15407,#15408,#15409,#15410,#15411,
#15412,#15413,#15414,#15415,#15416,#15417,#15418,#15419,#15420,#15421,#15422,
#15423,#15424,#15425,#15426,#15427,#15428),.UNSPECIFIED.,.F.,.F.,(4,3,3,
3,3,3,3,4),(-142.322100278399,-141.665286242036,-140.667643381176,-139.670000520317,
-138.672357659457,-137.674714798598,-136.677071937739,-136.03891497122),
 .UNSPECIFIED.);
#427=B_SPLINE_CURVE_WITH_KNOTS('',3,(#15429,#15430,#15431,#15432,#15433,
#15434,#15435,#15436,#15437,#15438,#15439,#15440,#15441,#15442,#15443,#15444,
#15445,#15446,#15447,#15448,#15449,#15450),.UNSPECIFIED.,.F.,.F.,(4,3,3,
3,3,3,3,4),(133.069633257233,133.73766567062,134.735707951744,135.733750232868,
136.731792513992,137.729834795116,138.72787707624,139.352818564412),
 .UNSPECIFIED.);
#428=B_SPLINE_CURVE_WITH_KNOTS('',3,(#15455,#15456,#15457,#15458,#15459,
#15460,#15461,#15462,#15463,#15464,#15465,#15466,#15467,#15468,#15469,#15470,
#15471,#15472,#15473,#15474,#15475,#15476),.UNSPECIFIED.,.F.,.F.,(4,3,3,
3,3,3,3,4),(-148.605285585579,-147.651143407192,-146.653500546333,-145.655857685473,
-144.658214824614,-143.660571963754,-142.662929102895,-142.322100278399),
 .UNSPECIFIED.);
#429=B_SPLINE_CURVE_WITH_KNOTS('',3,(#15477,#15478,#15479,#15480,#15481,
#15482,#15483,#15484,#15485,#15486,#15487,#15488,#15489,#15490,#15491,#15492,
#15493,#15494,#15495,#15496,#15497,#15498),.UNSPECIFIED.,.F.,.F.,(4,3,3,
3,3,3,3,4),(139.352818564412,139.725919357364,140.723961638488,141.722003919612,
142.720046200736,143.71808848186,144.716130762984,145.636003871592),
 .UNSPECIFIED.);
#430=B_SPLINE_CURVE_WITH_KNOTS('',3,(#15503,#15504,#15505,#15506,#15507,
#15508,#15509,#15510,#15511,#15512,#15513,#15514,#15515,#15516,#15517,#15518,
#15519,#15520,#15521,#15522,#15523,#15524,#15525,#15526,#15527),
 .UNSPECIFIED.,.F.,.F.,(4,3,3,3,3,3,3,3,4),(-154.888470892759,-154.634643433208,
-153.637000572349,-152.639357711489,-151.64171485063,-150.64407198977,-149.646429128911,
-148.648786268052,-148.605285585579),.UNSPECIFIED.);
#431=B_SPLINE_CURVE_WITH_KNOTS('',3,(#15528,#15529,#15530,#15531,#15532,
#15533,#15534,#15535,#15536,#15537,#15538,#15539,#15540,#15541,#15542,#15543,
#15544,#15545,#15546,#15547,#15548,#15549,#15550,#15551,#15552),
 .UNSPECIFIED.,.F.,.F.,(4,3,3,3,3,3,3,3,4),(145.636003871592,145.714173044108,
146.712215325232,147.710257606356,148.70829988748,149.706342168604,150.704384449728,
151.702426730852,151.919189178771),.UNSPECIFIED.);
#432=B_SPLINE_CURVE_WITH_KNOTS('',3,(#15557,#15558,#15559,#15560,#15561,
#15562,#15563,#15564,#15565,#15566,#15567,#15568,#15569,#15570,#15571,#15572,
#15573,#15574,#15575,#15576,#15577,#15578),.UNSPECIFIED.,.F.,.F.,(4,3,3,
3,3,3,3,4),(-161.171656199938,-160.620500598364,-159.622857737505,-158.625214876646,
-157.627572015786,-156.629929154927,-155.632286294067,-154.888470892759),
 .UNSPECIFIED.);
#433=B_SPLINE_CURVE_WITH_KNOTS('',3,(#15579,#15580,#15581,#15582,#15583,
#15584,#15585,#15586,#15587,#15588,#15589,#15590,#15591,#15592,#15593,#15594,
#15595,#15596,#15597,#15598,#15599,#15600),.UNSPECIFIED.,.F.,.F.,(4,3,3,
3,3,3,3,4),(151.919189178771,152.700469011976,153.6985112931,154.696553574224,
155.694595855348,156.692638136472,157.690680417596,158.202374485951),
 .UNSPECIFIED.);
#434=B_SPLINE_CURVE_WITH_KNOTS('',3,(#15605,#15606,#15607,#15608,#15609,
#15610,#15611,#15612,#15613,#15614,#15615,#15616,#15617,#15618,#15619,#15620,
#15621,#15622,#15623,#15624,#15625,#15626),.UNSPECIFIED.,.F.,.F.,(4,3,3,
3,3,3,3,4),(-167.454841507118,-166.606357763521,-165.608714902661,-164.611072041802,
-163.613429180943,-162.615786320083,-161.618143459224,-161.171656199938),
 .UNSPECIFIED.);
#435=B_SPLINE_CURVE_WITH_KNOTS('',3,(#15627,#15628,#15629,#15630,#15631,
#15632,#15633,#15634,#15635,#15636,#15637,#15638,#15639,#15640,#15641,#15642,
#15643,#15644,#15645,#15646,#15647,#15648),.UNSPECIFIED.,.F.,.F.,(4,3,3,
3,3,3,3,4),(158.202374485951,158.68872269872,159.686764979844,160.684807260968,
161.682849542092,162.680891823216,163.67893410434,164.48555979313),
 .UNSPECIFIED.);
#436=B_SPLINE_CURVE_WITH_KNOTS('',3,(#15653,#15654,#15655,#15656,#15657,
#15658,#15659,#15660,#15661,#15662,#15663,#15664,#15665,#15666,#15667,#15668,
#15669,#15670,#15671,#15672,#15673,#15674,#15675,#15676,#15677),
 .UNSPECIFIED.,.F.,.F.,(4,3,3,3,3,3,3,3,4),(-173.738026814297,-173.589857789537,
-172.592214928677,-171.594572067818,-170.596929206958,-169.599286346099,
-168.60164348524,-167.60400062438,-167.454841507118),.UNSPECIFIED.);
#437=B_SPLINE_CURVE_WITH_KNOTS('',3,(#15678,#15679,#15680,#15681,#15682,
#15683,#15684,#15685,#15686,#15687,#15688,#15689,#15690,#15691,#15692,#15693,
#15694,#15695,#15696,#15697,#15698,#15699,#15700,#15701,#15702),
 .UNSPECIFIED.,.F.,.F.,(4,3,3,3,3,3,3,3,4),(164.48555979313,164.676976385465,
165.675018666588,166.673060947713,167.671103228837,168.669145509961,169.667187791085,
170.665230072209,170.76874510031),.UNSPECIFIED.);
#438=B_SPLINE_CURVE_WITH_KNOTS('',3,(#15707,#15708,#15709,#15710,#15711,
#15712,#15713,#15714,#15715,#15716,#15717,#15718,#15719,#15720,#15721,#15722,
#15723,#15724,#15725,#15726,#15727,#15728),.UNSPECIFIED.,.F.,.F.,(4,3,3,
3,3,3,3,4),(-180.021212121477,-179.575714954693,-178.578072093834,-177.580429232974,
-176.582786372115,-175.585143511255,-174.587500650396,-173.738026814297),
 .UNSPECIFIED.);
#439=B_SPLINE_CURVE_WITH_KNOTS('',3,(#15729,#15730,#15731,#15732,#15733,
#15734,#15735,#15736,#15737,#15738,#15739,#15740,#15741,#15742,#15743,#15744,
#15745,#15746,#15747,#15748,#15749,#15750),.UNSPECIFIED.,.F.,.F.,(4,3,3,
3,3,3,3,4),(170.76874510031,171.663272353333,172.661314634457,173.659356915581,
174.657399196705,175.655441477829,176.653483758953,177.051930407489),
 .UNSPECIFIED.);
#440=B_SPLINE_CURVE_WITH_KNOTS('',3,(#15755,#15756,#15757,#15758,#15759,
#15760,#15761,#15762,#15763,#15764,#15765,#15766,#15767,#15768,#15769,#15770,
#15771,#15772,#15773,#15774,#15775,#15776),.UNSPECIFIED.,.F.,.F.,(4,3,3,
3,3,3,3,4),(-186.304397428656,-185.56157211985,-184.56392925899,-183.566286398131,
-182.568643537271,-181.571000676412,-180.573357815553,-180.021212121477),
 .UNSPECIFIED.);
#441=B_SPLINE_CURVE_WITH_KNOTS('',3,(#15777,#15778,#15779,#15780,#15781,
#15782,#15783,#15784,#15785,#15786,#15787,#15788,#15789,#15790,#15791,#15792,
#15793,#15794,#15795,#15796,#15797,#15798),.UNSPECIFIED.,.F.,.F.,(4,3,3,
3,3,3,3,4),(177.051930407489,177.651526040077,178.649568321201,179.647610602325,
180.645652883449,181.643695164573,182.641737445697,183.335115714669),
 .UNSPECIFIED.);
#442=B_SPLINE_CURVE_WITH_KNOTS('',3,(#15804,#15805,#15806,#15807,#15808,
#15809,#15810,#15811,#15812,#15813),.UNSPECIFIED.,.F.,.F.,(4,1,1,1,1,1,
1,4),(197.920337176157,198.17515472821,199.172797589069,200.170440449928,
201.168083310788,202.165726171647,203.163369032507,204.161011893366),
 .UNSPECIFIED.);
#443=B_SPLINE_CURVE_WITH_KNOTS('',3,(#15816,#15817,#15818,#15819,#15820,
#15821,#15822,#15823,#15824),.UNSPECIFIED.,.F.,.F.,(4,1,1,1,1,1,4),(197.920337176157,
197.930069567874,198.928111848998,199.926154130122,200.924196411246,201.92223869237,
202.920280973494),.UNSPECIFIED.);
#444=B_SPLINE_CURVE_WITH_KNOTS('',3,(#15829,#15830,#15831,#15832,#15833,
#15834,#15835,#15836,#15837,#15838),.UNSPECIFIED.,.F.,.F.,(4,1,1,1,1,1,
1,4),(191.637151868977,192.189297563053,193.186940423913,194.184583284772,
195.182226145631,196.179869006491,197.17751186735,197.920337176157),
 .UNSPECIFIED.);
#445=B_SPLINE_CURVE_WITH_KNOTS('',3,(#15839,#15840,#15841,#15842,#15843,
#15844,#15845,#15846,#15847,#15848),.UNSPECIFIED.,.F.,.F.,(4,1,1,1,1,1,
1,4),(191.637151868977,191.94181588113,192.939858162254,193.937900443378,
194.935942724502,195.933985005626,196.93202728675,197.920337176157),
 .UNSPECIFIED.);
#446=B_SPLINE_CURVE_WITH_KNOTS('',3,(#15853,#15854,#15855,#15856,#15857,
#15858,#15859,#15860,#15861,#15862),.UNSPECIFIED.,.F.,.F.,(4,1,1,1,1,1,
1,4),(185.353966561798,186.203440397897,187.201083258756,188.198726119616,
189.196368980475,190.194011841334,191.191654702194,191.637151868977),
 .UNSPECIFIED.);
#447=B_SPLINE_CURVE_WITH_KNOTS('',3,(#15863,#15864,#15865,#15866,#15867,
#15868,#15869,#15870,#15871,#15872),.UNSPECIFIED.,.F.,.F.,(4,1,1,1,1,1,
1,4),(185.353966561798,185.953562194385,186.951604475509,187.949646756633,
188.947689037757,189.945731318881,190.943773600006,191.637151868977),
 .UNSPECIFIED.);
#448=B_SPLINE_CURVE_WITH_KNOTS('',3,(#15877,#15878,#15879,#15880,#15881,
#15882,#15883,#15884,#15885,#15886,#15887),.UNSPECIFIED.,.F.,.F.,(4,1,1,
1,1,1,1,1,4),(179.070781254618,179.219940371881,180.21758323274,181.2152260936,
182.212868954459,183.210511815318,184.208154676178,185.205797537037,185.353966561798),
 .UNSPECIFIED.);
#449=B_SPLINE_CURVE_WITH_KNOTS('',3,(#15888,#15889,#15890,#15891,#15892,
#15893,#15894,#15895,#15896,#15897),.UNSPECIFIED.,.F.,.F.,(4,1,1,1,1,1,
1,4),(179.070781254618,179.965308507641,180.963350788765,181.961393069889,
182.959435351013,183.957477632137,184.955519913261,185.353966561798),
 .UNSPECIFIED.);
#450=B_SPLINE_CURVE_WITH_KNOTS('',3,(#15902,#15903,#15904,#15905,#15906,
#15907,#15908,#15909,#15910,#15911),.UNSPECIFIED.,.F.,.F.,(4,1,1,1,1,1,
1,4),(172.787595947439,173.234083206724,174.231726067584,175.229368928443,
176.227011789303,177.224654650162,178.222297511021,179.070781254618),
 .UNSPECIFIED.);
#451=B_SPLINE_CURVE_WITH_KNOTS('',3,(#15912,#15913,#15914,#15915,#15916,
#15917,#15918,#15919,#15920,#15921,#15922),.UNSPECIFIED.,.F.,.F.,(4,1,1,
1,1,1,1,1,4),(172.787595947439,172.979012539773,173.977054820897,174.975097102021,
175.973139383145,176.971181664269,177.969223945393,178.967266226517,179.070781254618),
 .UNSPECIFIED.);
#452=B_SPLINE_CURVE_WITH_KNOTS('',3,(#15927,#15928,#15929,#15930,#15931,
#15932,#15933,#15934,#15935,#15936),.UNSPECIFIED.,.F.,.F.,(4,1,1,1,1,1,
1,4),(166.504410640259,167.248226041568,168.245868902427,169.243511763287,
170.241154624146,171.238797485006,172.236440345865,172.787595947439),
 .UNSPECIFIED.);
#453=B_SPLINE_CURVE_WITH_KNOTS('',3,(#15937,#15938,#15939,#15940,#15941,
#15942,#15943,#15944,#15945,#15946),.UNSPECIFIED.,.F.,.F.,(4,1,1,1,1,1,
1,4),(166.504410640259,166.990758853029,167.988801134153,168.986843415277,
169.984885696401,170.982927977525,171.980970258649,172.787595947439),
 .UNSPECIFIED.);
#454=B_SPLINE_CURVE_WITH_KNOTS('',3,(#15951,#15952,#15953,#15954,#15955,
#15956,#15957,#15958,#15959,#15960,#15961),.UNSPECIFIED.,.F.,.F.,(4,1,1,
1,1,1,1,1,4),(160.22122533308,160.264726015552,161.262368876412,162.260011737271,
163.25765459813,164.25529745899,165.252940319849,166.250583180709,166.504410640259),
 .UNSPECIFIED.);
#455=B_SPLINE_CURVE_WITH_KNOTS('',3,(#15962,#15963,#15964,#15965,#15966,
#15967,#15968,#15969,#15970,#15971),.UNSPECIFIED.,.F.,.F.,(4,1,1,1,1,1,
1,4),(160.22122533308,161.002505166285,162.000547447409,162.998589728533,
163.996632009657,164.994674290781,165.992716571905,166.504410640259),
 .UNSPECIFIED.);
#456=B_SPLINE_CURVE_WITH_KNOTS('',3,(#15976,#15977,#15978,#15979,#15980,
#15981,#15982,#15983,#15984,#15985),.UNSPECIFIED.,.F.,.F.,(4,1,1,1,1,1,
1,4),(153.9380400259,154.278868850396,155.276511711255,156.274154572115,
157.271797432974,158.269440293833,159.267083154693,160.22122533308),
 .UNSPECIFIED.);
#457=B_SPLINE_CURVE_WITH_KNOTS('',3,(#15986,#15987,#15988,#15989,#15990,
#15991,#15992,#15993,#15994,#15995,#15996),.UNSPECIFIED.,.F.,.F.,(4,1,1,
1,1,1,1,1,4),(153.9380400259,154.016209198417,155.014251479541,156.012293760665,
157.010336041789,158.008378322913,159.006420604037,160.004462885161,160.22122533308),
 .UNSPECIFIED.);
#458=B_SPLINE_CURVE_WITH_KNOTS('',3,(#16001,#16002,#16003,#16004,#16005,
#16006,#16007,#16008,#16009,#16010),.UNSPECIFIED.,.F.,.F.,(4,1,1,1,1,1,
1,4),(147.65485471872,148.293011685239,149.290654546099,150.288297406958,
151.285940267817,152.283583128677,153.281225989536,153.9380400259),
 .UNSPECIFIED.);
#459=B_SPLINE_CURVE_WITH_KNOTS('',3,(#16011,#16012,#16013,#16014,#16015,
#16016,#16017,#16018,#16019,#16020),.UNSPECIFIED.,.F.,.F.,(4,1,1,1,1,1,
1,4),(147.65485471872,148.027955511672,149.025997792796,150.02404007392,
151.022082355044,152.020124636168,153.018166917292,153.9380400259),
 .UNSPECIFIED.);
#460=B_SPLINE_CURVE_WITH_KNOTS('',3,(#16025,#16026,#16027,#16028,#16029,
#16030,#16031,#16032,#16033,#16034),.UNSPECIFIED.,.F.,.F.,(4,1,1,1,1,1,
1,4),(141.371669411541,142.307154520083,143.304797380942,144.302440241802,
145.300083102661,146.29772596352,147.29536882438,147.65485471872),
 .UNSPECIFIED.);
#461=B_SPLINE_CURVE_WITH_KNOTS('',3,(#16035,#16036,#16037,#16038,#16039,
#16040,#16041,#16042,#16043,#16044),.UNSPECIFIED.,.F.,.F.,(4,1,1,1,1,1,
1,4),(141.371669411541,142.039701824928,143.037744106052,144.035786387176,
145.0338286683,146.031870949424,147.029913230548,147.65485471872),
 .UNSPECIFIED.);
#462=B_SPLINE_CURVE_WITH_KNOTS('',3,(#16049,#16050,#16051,#16052,#16053,
#16054,#16055,#16056,#16057,#16058,#16059),.UNSPECIFIED.,.F.,.F.,(4,1,1,
1,1,1,1,1,4),(135.088484104361,135.323654494067,136.321297354926,137.318940215786,
138.316583076645,139.314225937505,140.311868798364,141.309511659223,141.371669411541),
 .UNSPECIFIED.);
#463=B_SPLINE_CURVE_WITH_KNOTS('',3,(#16060,#16061,#16062,#16063,#16064,
#16065,#16066,#16067,#16068,#16069),.UNSPECIFIED.,.F.,.F.,(4,1,1,1,1,1,
1,4),(135.088484104361,136.051448138184,137.049490419308,138.047532700432,
139.045574981556,140.04361726268,141.041659543804,141.371669411541),
 .UNSPECIFIED.);
#464=B_SPLINE_CURVE_WITH_KNOTS('',3,(#16074,#16075,#16076,#16077,#16078,
#16079,#16080,#16081,#16082,#16083),.UNSPECIFIED.,.F.,.F.,(4,1,1,1,1,1,
1,4),(128.805298797182,129.337797328911,130.33544018977,131.333083050629,
132.330725911489,133.328368772348,134.326011633208,135.088484104361),
 .UNSPECIFIED.);
#465=B_SPLINE_CURVE_WITH_KNOTS('',3,(#16084,#16085,#16086,#16087,#16088,
#16089,#16090,#16091,#16092,#16093,#16094),.UNSPECIFIED.,.F.,.F.,(4,1,1,
1,1,1,1,1,4),(128.805298797182,129.065152170316,130.06319445144,131.061236732564,
132.059279013688,133.057321294812,134.055363575936,135.05340585706,135.088484104361),
 .UNSPECIFIED.);
#466=B_SPLINE_CURVE_WITH_KNOTS('',3,(#16099,#16100,#16101,#16102,#16103,
#16104,#16105,#16106,#16107,#16108),.UNSPECIFIED.,.F.,.F.,(4,1,1,1,1,1,
1,4),(122.522113490002,123.351940163754,124.349583024614,125.347225885473,
126.344868746332,127.342511607192,128.340154468051,128.805298797182),
 .UNSPECIFIED.);
#467=B_SPLINE_CURVE_WITH_KNOTS('',3,(#16109,#16110,#16111,#16112,#16113,
#16114,#16115,#16116,#16117,#16118),.UNSPECIFIED.,.F.,.F.,(4,1,1,1,1,1,
1,4),(122.522113490002,123.076898483572,124.074940764696,125.07298304582,
126.071025326944,127.069067608068,128.067109889192,128.805298797182),
 .UNSPECIFIED.);
#468=B_SPLINE_CURVE_WITH_KNOTS('',3,(#16123,#16124,#16125,#16126,#16127,
#16128,#16129,#16130,#16131,#16132,#16133),.UNSPECIFIED.,.F.,.F.,(4,1,1,
1,1,1,1,1,4),(116.238928182823,116.368440137738,117.366082998598,118.363725859457,
119.361368720316,120.359011581176,121.356654442035,122.354297302895,122.522113490002),
 .UNSPECIFIED.);
#469=B_SPLINE_CURVE_WITH_KNOTS('',3,(#16134,#16135,#16136,#16137,#16138,
#16139,#16140,#16141,#16142,#16143),.UNSPECIFIED.,.F.,.F.,(4,1,1,1,1,1,
1,4),(116.238928182823,117.088644796828,118.086687077952,119.084729359076,
120.0827716402,121.080813921324,122.078856202448,122.522113490002),
 .UNSPECIFIED.);
#470=B_SPLINE_CURVE_WITH_KNOTS('',3,(#16148,#16149,#16150,#16151,#16152,
#16153,#16154,#16155,#16156,#16157),.UNSPECIFIED.,.F.,.F.,(4,1,1,1,1,1,
1,4),(109.955742875643,110.382582972582,111.380225833441,112.377868694301,
113.37551155516,114.373154416019,115.370797276879,116.238928182823),
 .UNSPECIFIED.);
#471=B_SPLINE_CURVE_WITH_KNOTS('',3,(#16158,#16159,#16160,#16161,#16162,
#16163,#16164,#16165,#16166,#16167,#16168),.UNSPECIFIED.,.F.,.F.,(4,1,1,
1,1,1,1,1,4),(109.955742875643,110.102348828959,111.100391110083,112.098433391207,
113.096475672331,114.094517953455,115.092560234579,116.090602515703,116.238928182823),
 .UNSPECIFIED.);
#472=B_SPLINE_CURVE_WITH_KNOTS('',3,(#16173,#16174,#16175,#16176,#16177,
#16178,#16179,#16180,#16181,#16182),.UNSPECIFIED.,.F.,.F.,(4,1,1,1,1,1,
1,4),(103.672557568463,104.396725807425,105.394368668285,106.392011529144,
107.389654390004,108.387297250863,109.384940111722,109.955742875643),
 .UNSPECIFIED.);
#473=B_SPLINE_CURVE_WITH_KNOTS('',3,(#16183,#16184,#16185,#16186,#16187,
#16188,#16189,#16190,#16191,#16192),.UNSPECIFIED.,.F.,.F.,(4,1,1,1,1,1,
1,4),(103.672557568463,104.114095142215,105.112137423339,106.110179704463,
107.108221985587,108.106264266711,109.104306547835,109.955742875643),
 .UNSPECIFIED.);
#474=B_SPLINE_CURVE_WITH_KNOTS('',3,(#16197,#16198,#16199,#16200,#16201,
#16202,#16203,#16204,#16205,#16206,#16207),.UNSPECIFIED.,.F.,.F.,(4,1,1,
1,1,1,1,1,4),(97.3893722612837,97.4132257814096,98.410868642269,99.4085115031284,
100.406154363988,101.403797224847,102.401440085707,103.399082946566,103.672557568463),
 .UNSPECIFIED.);
#475=B_SPLINE_CURVE_WITH_KNOTS('',3,(#16208,#16209,#16210,#16211,#16212,
#16213,#16214,#16215,#16216,#16217),.UNSPECIFIED.,.F.,.F.,(4,1,1,1,1,1,
1,4),(97.3893722612838,98.125841455471,99.123883736595,100.121926017719,
101.119968298843,102.118010579967,103.116052861091,103.672557568463),
 .UNSPECIFIED.);
#476=B_SPLINE_CURVE_WITH_KNOTS('',3,(#16222,#16223,#16224,#16225,#16226,
#16227,#16228,#16229,#16230,#16231),.UNSPECIFIED.,.F.,.F.,(4,1,1,1,1,1,
1,4),(91.1061869541041,91.4273686162531,92.4250114771125,93.4226543379719,
94.4202971988313,95.4179400596907,96.4155829205502,97.3893722612837),
 .UNSPECIFIED.);
#477=B_SPLINE_CURVE_WITH_KNOTS('',3,(#16232,#16233,#16234,#16235,#16236,
#16237,#16238,#16239,#16240,#16241,#16242),.UNSPECIFIED.,.F.,.F.,(4,1,1,
1,1,1,1,1,4),(91.1061869541042,91.1395454876028,92.1375877687268,93.1356300498508,
94.1336723309749,95.1317146120989,96.1297568932229,97.127799174347,97.3893722612838),
 .UNSPECIFIED.);
#478=B_SPLINE_CURVE_WITH_KNOTS('',3,(#16247,#16248,#16249,#16250,#16251,
#16252,#16253,#16254,#16255,#16256),.UNSPECIFIED.,.F.,.F.,(4,1,1,1,1,1,
1,4),(84.8230016469245,85.4415114510967,86.4391543119561,87.4367971728155,
88.4344400336749,89.4320828945343,90.4297257553937,91.1061869541041),
 .UNSPECIFIED.);
#479=B_SPLINE_CURVE_WITH_KNOTS('',3,(#16257,#16258,#16259,#16260,#16261,
#16262,#16263,#16264,#16265,#16266),.UNSPECIFIED.,.F.,.F.,(4,1,1,1,1,1,
1,4),(84.8230016469246,85.1512918008586,86.1493340819827,87.1473763631067,
88.1454186442307,89.1434609253548,90.1415032064788,91.1061869541042),
 .UNSPECIFIED.);
#480=B_SPLINE_CURVE_WITH_KNOTS('',3,(#16271,#16272,#16273,#16274,#16275,
#16276,#16277,#16278,#16279,#16280),.UNSPECIFIED.,.F.,.F.,(4,1,1,1,1,1,
1,4),(78.539816339745,79.4556542859402,80.4532971467996,81.4509400076591,
82.4485828685185,83.4462257293779,84.4438685902373,84.8230016469245),
 .UNSPECIFIED.);
#481=B_SPLINE_CURVE_WITH_KNOTS('',3,(#16281,#16282,#16283,#16284,#16285,
#16286,#16287,#16288,#16289,#16290),.UNSPECIFIED.,.F.,.F.,(4,1,1,1,1,1,
1,4),(78.539816339745,79.1630381141145,80.1610803952385,81.1591226763625,
82.1571649574865,83.1552072386106,84.1532495197346,84.8230016469246),
 .UNSPECIFIED.);
#482=B_SPLINE_CURVE_WITH_KNOTS('',3,(#16295,#16296,#16297,#16298,#16299,
#16300,#16301,#16302,#16303,#16304,#16305),.UNSPECIFIED.,.F.,.F.,(4,1,1,
1,1,1,1,1,4),(72.2566310325654,72.4721542599244,73.4697971207838,74.4674399816432,
75.4650828425026,76.462725703362,77.4603685642214,78.4580114250808,78.539816339745),
 .UNSPECIFIED.);
#483=B_SPLINE_CURVE_WITH_KNOTS('',3,(#16306,#16307,#16308,#16309,#16310,
#16311,#16312,#16313,#16314,#16315),.UNSPECIFIED.,.F.,.F.,(4,1,1,1,1,1,
1,4),(72.2566310325654,73.1747844273703,74.1728267084943,75.1708689896184,
76.1689112707424,77.1669535518664,78.1649958329905,78.539816339745),
 .UNSPECIFIED.);
#484=B_SPLINE_CURVE_WITH_KNOTS('',3,(#16320,#16321,#16322,#16323,#16324,
#16325,#16326,#16327,#16328,#16329),.UNSPECIFIED.,.F.,.F.,(4,1,1,1,1,1,
1,4),(65.9734457253858,66.486297094768,67.4839399556274,68.4815828164868,
69.4792256773462,70.4768685382056,71.474511399065,72.2566310325654),
 .UNSPECIFIED.);
#485=B_SPLINE_CURVE_WITH_KNOTS('',3,(#16330,#16331,#16332,#16333,#16334,
#16335,#16336,#16337,#16338,#16339,#16340),.UNSPECIFIED.,.F.,.F.,(4,1,1,
1,1,1,1,1,4),(65.9734457253858,66.1884884595021,67.1865307406262,68.1845730217502,
69.1826153028742,70.1806575839982,71.1786998651223,72.1767421462463,72.2566310325654),
 .UNSPECIFIED.);
#486=B_SPLINE_CURVE_WITH_KNOTS('',3,(#16345,#16346,#16347,#16348,#16349,
#16350,#16351,#16352,#16353,#16354),.UNSPECIFIED.,.F.,.F.,(4,1,1,1,1,1,
1,4),(59.6902604182062,60.5004399296115,61.4980827904709,62.4957256513303,
63.4933685121897,64.4910113730492,65.4886542339086,65.9734457253858),
 .UNSPECIFIED.);
#487=B_SPLINE_CURVE_WITH_KNOTS('',3,(#16355,#16356,#16357,#16358,#16359,
#16360,#16361,#16362,#16363,#16364),.UNSPECIFIED.,.F.,.F.,(4,1,1,1,1,1,
1,4),(59.6902604182062,60.200234772758,61.198277053882,62.196319335006,
63.19436161613,64.1924038972541,65.1904461783781,65.9734457253858),
 .UNSPECIFIED.);
#488=B_SPLINE_CURVE_WITH_KNOTS('',3,(#16369,#16370,#16371,#16372,#16373,
#16374,#16375,#16376,#16377,#16378,#16379),.UNSPECIFIED.,.F.,.F.,(4,1,1,
1,1,1,1,1,4),(53.4070751110266,53.5169399035957,54.5145827644551,55.5122256253145,
56.5098684861739,57.5075113470333,58.5051542078927,59.5027970687521,59.6902604182062),
 .UNSPECIFIED.);
#489=B_SPLINE_CURVE_WITH_KNOTS('',3,(#16380,#16381,#16382,#16383,#16384,
#16385,#16386,#16387,#16388,#16389),.UNSPECIFIED.,.F.,.F.,(4,1,1,1,1,1,
1,4),(53.4070751110266,54.2119810860138,55.2100233671378,56.2080656482619,
57.2061079293859,58.2041502105099,59.2021924916339,59.6902604182062),
 .UNSPECIFIED.);
#490=B_SPLINE_CURVE_WITH_KNOTS('',3,(#16394,#16395,#16396,#16397,#16398,
#16399,#16400,#16401,#16402,#16403),.UNSPECIFIED.,.F.,.F.,(4,1,1,1,1,1,
1,4),(47.123889803847,47.5310827384393,48.5287255992987,49.5263684601581,
50.5240113210175,51.5216541818769,52.5192970427363,53.4070751110266),
 .UNSPECIFIED.);
#491=B_SPLINE_CURVE_WITH_KNOTS('',3,(#16404,#16405,#16406,#16407,#16408,
#16409,#16410,#16411,#16412,#16413,#16414),.UNSPECIFIED.,.F.,.F.,(4,1,1,
1,1,1,1,1,4),(47.123889803847,47.2256851181456,48.2237273992696,49.2217696803937,
50.2198119615177,51.2178542426417,52.2158965237657,53.2139388048898,53.4070751110266),
 .UNSPECIFIED.);
#492=B_SPLINE_CURVE_WITH_KNOTS('',3,(#16419,#16420,#16421,#16422,#16423,
#16424,#16425,#16426,#16427,#16428),.UNSPECIFIED.,.F.,.F.,(4,1,1,1,1,1,
1,4),(40.8407044966674,41.5452255732828,42.5428684341422,43.5405112950016,
44.538154155861,45.5357970167204,46.5334398775799,47.123889803847),
 .UNSPECIFIED.);
#493=B_SPLINE_CURVE_WITH_KNOTS('',3,(#16429,#16430,#16431,#16432,#16433,
#16434,#16435,#16436,#16437,#16438),.UNSPECIFIED.,.F.,.F.,(4,1,1,1,1,1,
1,4),(40.8407044966675,41.2374314314014,42.2354737125255,43.2335159936495,
44.2315582747735,45.2296005558975,46.2276428370216,47.123889803847),
 .UNSPECIFIED.);
#494=B_SPLINE_CURVE_WITH_KNOTS('',3,(#16443,#16444,#16445,#16446,#16447,
#16448,#16449,#16450,#16451,#16452,#16453),.UNSPECIFIED.,.F.,.F.,(4,1,1,
1,1,1,1,1,4),(34.5575191894878,34.561725547267,35.5593684081264,36.5570112689858,
37.5546541298452,38.5522969907046,39.549939851564,40.5475827124234,40.8407044966674),
 .UNSPECIFIED.);
#495=B_SPLINE_CURVE_WITH_KNOTS('',3,(#16454,#16455,#16456,#16457,#16458,
#16459,#16460,#16461,#16462,#16463),.UNSPECIFIED.,.F.,.F.,(4,1,1,1,1,1,
1,4),(34.5575191894879,35.2491777446573,36.2472200257813,37.2452623069053,
38.2433045880294,39.2413468691534,40.2393891502774,40.8407044966675),
 .UNSPECIFIED.);
#496=B_SPLINE_CURVE_WITH_KNOTS('',3,(#16468,#16469,#16470,#16471,#16472,
#16473,#16474,#16475,#16476,#16477),.UNSPECIFIED.,.F.,.F.,(4,1,1,1,1,1,
1,4),(28.2743338823082,28.5758683821105,29.5735112429699,30.5711541038294,
31.5687969646888,32.5664398255482,33.5640826864076,34.5575191894878),
 .UNSPECIFIED.);
#497=B_SPLINE_CURVE_WITH_KNOTS('',3,(#16478,#16479,#16480,#16481,#16482,
#16483,#16484,#16485,#16486,#16487),.UNSPECIFIED.,.F.,.F.,(4,1,1,1,1,1,
1,4),(28.2743338823083,29.2609240579131,30.2589663390371,31.2570086201612,
32.2550509012852,33.2530931824092,34.2511354635333,34.5575191894879),
 .UNSPECIFIED.);
#498=B_SPLINE_CURVE_WITH_KNOTS('',3,(#16492,#16493,#16494,#16495,#16496,
#16497,#16498,#16499,#16500,#16501),.UNSPECIFIED.,.F.,.F.,(4,1,1,1,1,1,
1,4),(21.9911485751286,22.5900112169541,23.5876540778135,24.5852969386729,
25.5829397995323,26.5805826603917,27.5782255212511,28.2743338823082),
 .UNSPECIFIED.);
#499=B_SPLINE_CURVE_WITH_KNOTS('',3,(#16502,#16503,#16504,#16505,#16506,
#16507,#16508,#16509,#16510,#16511,#16512),.UNSPECIFIED.,.F.,.F.,(4,1,1,
1,1,1,1,1,4),(21.9911485751287,22.2746280900449,23.272670371169,24.270712652293,
25.268754933417,26.266797214541,27.2648394956651,28.2628817767891,28.2743338823083),
 .UNSPECIFIED.);
#500=B_SPLINE_CURVE_WITH_KNOTS('',3,(#16517,#16518,#16519,#16520,#16521,
#16522,#16523,#16524,#16525,#16526),.UNSPECIFIED.,.F.,.F.,(4,1,1,1,1,1,
1,4),(15.707963267949,16.6041540517977,17.6017969126571,18.5994397735165,
19.5970826343759,20.5947254952353,21.5923683560947,21.9911485751286),
 .UNSPECIFIED.);
#501=B_SPLINE_CURVE_WITH_KNOTS('',3,(#16527,#16528,#16529,#16530,#16531,
#16532,#16533,#16534,#16535,#16536),.UNSPECIFIED.,.F.,.F.,(4,1,1,1,1,1,
1,4),(15.7079632679491,16.2863744033008,17.2844166844248,18.2824589655488,
19.2805012466728,20.2785435277969,21.2765858089209,21.9911485751287),
 .UNSPECIFIED.);
#502=B_SPLINE_CURVE_WITH_KNOTS('',3,(#16539,#16540,#16541,#16542,#16543,
#16544,#16545,#16546,#16547,#16548,#16549,#16550,#16551,#16552,#16553,#16554,
#16555,#16556,#16557,#16558,#16559,#16560,#16561,#16562,#16563,#16564,#16565,
#16566,#16567,#16568,#16569,#16570,#16571,#16572,#16573,#16574,#16575,#16576,
#16577,#16578,#16579,#16580,#16581,#16582,#16583,#16584,#16585,#16586,#16587,
#16588,#16589,#16590,#16591,#16592,#16593,#16594,#16595,#16596,#16597,#16598,
#16599,#16600,#16601,#16602,#16603,#16604,#16605,#16606,#16607,#16608,#16609,
#16610,#16611,#16612,#16613,#16614,#16615,#16616,#16617,#16618,#16619,#16620,
#16621,#16622,#16623,#16624,#16625,#16626,#16627,#16628,#16629,#16630,#16631,
#16632,#16633,#16634,#16635,#16636,#16637,#16638,#16639,#16640,#16641,#16642,
#16643,#16644,#16645,#16646,#16647,#16648,#16649,#16650,#16651,#16652,#16653,
#16654,#16655,#16656,#16657,#16658,#16659),.UNSPECIFIED.,.F.,.F.,(4,3,3,
3,3,3,3,3,3,3,3,3,3,3,3,3,3,3,3,3,3,3,3,3,3,3,3,3,3,3,3,3,3,3,3,3,3,3,3,
3,4),(-0.753008129282056,-0.726412283548368,-0.715911613874471,-0.694893371653716,
-0.683361029549332,-0.673826434412814,-0.652889016486892,-0.639679181765185,
-0.63195159856097,-0.60480408471638,-0.59150990338668,-0.582561183693184,
-0.554067746128576,-0.540494882749548,-0.528208608719221,-0.505843484121927,
-0.4921308028701,-0.483102814228457,-0.456032674248847,-0.436199115577779,
-0.427073928162626,-0.400948091236321,-0.382860905241332,-0.374822254310016,
-0.34584221065474,-0.333939649620793,-0.324058619604945,-0.29393738163796,
-0.278576588250954,-0.269234263278142,-0.238815915606663,-0.225742435796944,
-0.216239773488962,-0.18666367230127,-0.170750005528772,-0.161294486761502,
-0.129614927749849,-0.114924930935507,-0.106250072717365,-0.0979353687381955,
-0.0965360155478562),.UNSPECIFIED.);
#503=B_SPLINE_CURVE_WITH_KNOTS('',3,(#16661,#16662,#16663,#16664,#16665,
#16666,#16667,#16668,#16669,#16670,#16671,#16672,#16673,#16674,#16675,#16676,
#16677,#16678,#16679,#16680,#16681,#16682,#16683,#16684,#16685,#16686,#16687,
#16688,#16689,#16690,#16691,#16692,#16693,#16694,#16695,#16696,#16697),
 .UNSPECIFIED.,.F.,.F.,(4,3,3,3,3,3,3,3,3,3,3,3,4),(-0.204609524178132,
-0.173922074105667,-0.152149392827302,-0.142793959810126,-0.12983323009626,
-0.11308637627832,-0.0998536142809363,-0.090547498816978,-0.0679106241127335,
-0.0514558350659385,-0.042025593252969,-0.0155529233063705,0.),
 .UNSPECIFIED.);
#504=B_SPLINE_CURVE_WITH_KNOTS('',3,(#16700,#16701,#16702,#16703,#16704,
#16705,#16706,#16707,#16708,#16709,#16710,#16711,#16712,#16713,#16714,#16715),
 .UNSPECIFIED.,.F.,.F.,(4,3,3,3,3,4),(-0.0965360155478562,-0.0724020116608921,
-0.0590232605257019,-0.050388474335024,-0.0186937936910934,0.),
 .UNSPECIFIED.);
#505=B_SPLINE_CURVE_WITH_KNOTS('',3,(#17504,#17505,#17506,#17507,#17508,
#17509,#17510,#17511),.UNSPECIFIED.,.F.,.F.,(4,1,1,1,1,4),(11.6159397475006,
12.61358260836,13.6112254692194,14.6088683300789,15.6065111909383,15.707963267949),
 .UNSPECIFIED.);
#506=B_SPLINE_CURVE_WITH_KNOTS('',3,(#17512,#17513,#17514,#17515,#17516,
#17517,#17518,#17519,#17520,#17521,#17522,#17523,#17524,#17525,#17526,#17527,
#17528,#17529,#17530,#17531,#17532,#17533,#17534,#17535,#17536,#17537,#17538,
#17539,#17540,#17541,#17542,#17543,#17544,#17545,#17546,#17547,#17548,#17549,
#17550,#17551,#17552,#17553,#17554,#17555,#17556,#17557,#17558,#17559,#17560),
 .UNSPECIFIED.,.F.,.F.,(4,3,3,3,3,3,3,3,3,3,3,3,3,3,3,3,4),(-0.275362278356892,
-0.263988733943187,-0.242277787653762,-0.228409792083558,-0.208856161945484,
-0.197709057767663,-0.168075464588018,-0.150222803571495,-0.140083955862437,
-0.125365894046572,-0.0997819296507484,-0.0889593225835958,-0.0667194919376969,
-0.0511923416312717,-0.0404361839568205,-0.0141940669149386,0.),
 .UNSPECIFIED.);
#507=B_SPLINE_CURVE_WITH_KNOTS('',3,(#17561,#17562,#17563,#17564,#17565,
#17566,#17567,#17568,#17569,#17570,#17571,#17572,#17573,#17574,#17575,#17576,
#17577,#17578,#17579),.UNSPECIFIED.,.F.,.F.,(4,3,3,3,3,3,4),(-191.027404416132,
-190.549786424147,-189.552143563287,-188.554500702428,-187.556857841568,
-186.559214980709,-186.304397428656),.UNSPECIFIED.);
#508=B_SPLINE_CURVE_WITH_KNOTS('',3,(#17582,#17583,#17584,#17585,#17586,
#17587,#17588,#17589,#17590),.UNSPECIFIED.,.F.,.F.,(4,1,1,1,1,1,4),(10.3752088276283,
11.2961629976806,12.2942052788047,13.2922475599287,14.2902898410527,15.2883321221767,
15.7079632679491),.UNSPECIFIED.);
#509=B_SPLINE_CURVE_WITH_KNOTS('',3,(#18384,#18385,#18386,#18387,#18388,
#18389,#18390,#18391,#18392,#18393,#18394,#18395,#18396,#18397,#18398,#18399,
#18400,#18401,#18402,#18403,#18404,#18405),.UNSPECIFIED.,.F.,.F.,(4,3,3,
3,3,3,3,4),(183.335115714669,183.639779726821,184.637822007945,185.635864289069,
186.633906570193,187.631948851317,188.629991132441,188.954231742812),
 .UNSPECIFIED.);
#510=B_SPLINE_CURVE_WITH_KNOTS('',3,(#18406,#18407,#18408,#18409,#18410,
#18411,#18412,#18413,#18414,#18415,#18416,#18417,#18418,#18419,#18420,#18421,
#18422,#18423,#18424,#18425,#18426,#18427,#18428,#18429,#18430,#18431,#18432,
#18433,#18434,#18435,#18436,#18437,#18438,#18439,#18440,#18441,#18442,#18443,
#18444,#18445,#18446,#18447,#18448,#18449,#18450,#18451,#18452,#18453,#18454,
#18455,#18456,#18457),.UNSPECIFIED.,.F.,.F.,(4,3,3,3,3,3,3,3,3,3,3,3,3,
3,3,3,3,4),(-0.276631791712714,-0.267404104599176,-0.245529112929484,-0.233826742508505,
-0.212230201958684,-0.201819484750363,-0.173281546649687,-0.162756755581661,
-0.152537502224722,-0.140478169692516,-0.120739781640826,-0.110641775261762,
-0.100726383882944,-0.0755447879122082,-0.0587891884452614,-0.0493012364577666,
-0.0182848522583483,0.),.UNSPECIFIED.);
#511=B_SPLINE_CURVE_WITH_KNOTS('',3,(#18512,#18513,#18514,#18515,#18516,
#18517,#18518),.UNSPECIFIED.,.F.,.F.,(4,3,4),(-30.159289474462,-29.2544199692899,
-28.9853432330879),.UNSPECIFIED.);
#512=B_SPLINE_CURVE_WITH_KNOTS('',3,(#18524,#18525,#18526,#18527,#18528,
#18529,#18530,#18531,#18532,#18533,#18534,#18535,#18536,#18537,#18538,#18539,
#18540,#18541,#18542),.UNSPECIFIED.,.F.,.F.,(4,3,3,3,3,3,4),(26.4423043696954,
27.3041253046706,28.2792726369803,29.25441996929,30.2295673015996,31.2047146339093,
32.179861966219),.UNSPECIFIED.);
#513=B_SPLINE_CURVE_WITH_KNOTS('',3,(#18544,#18545,#18546,#18547,#18548,
#18549,#18550,#18551,#18552,#18553,#18554,#18555,#18556,#18557,#18558,#18559,
#18560,#18561,#18562,#18563,#18564,#18565),.UNSPECIFIED.,.F.,.F.,(4,3,3,
3,3,3,3,4),(-28.9853432330879,-28.2792726369803,-27.3041253046706,-26.3289779723609,
-25.3538306400513,-24.3786833077416,-23.403535975432,-22.7021579259084),
 .UNSPECIFIED.);
#514=B_SPLINE_CURVE_WITH_KNOTS('',3,(#18570,#18571,#18572,#18573,#18574,
#18575,#18576,#18577,#18578,#18579,#18580,#18581,#18582,#18583,#18584,#18585,
#18586,#18587,#18588,#18589,#18590,#18591,#18592,#18593,#18594),
 .UNSPECIFIED.,.F.,.F.,(4,3,3,3,3,3,3,3,4),(20.1591190625159,20.478093978503,
21.4532413108126,22.4283886431223,23.403535975432,24.3786833077416,25.3538306400513,
26.328977972361,26.4423043696954),.UNSPECIFIED.);
#515=B_SPLINE_CURVE_WITH_KNOTS('',3,(#18595,#18596,#18597,#18598,#18599,
#18600,#18601,#18602,#18603,#18604,#18605,#18606,#18607,#18608,#18609,#18610,
#18611,#18612,#18613,#18614,#18615,#18616,#18617,#18618,#18619),
 .UNSPECIFIED.,.F.,.F.,(4,3,3,3,3,3,3,3,4),(-22.7021579259084,-22.4283886431223,
-21.4532413108126,-20.478093978503,-19.5029466461933,-18.5277993138836,
-17.552651981574,-16.5775046492643,-16.4189726187288),.UNSPECIFIED.);
#516=B_SPLINE_CURVE_WITH_KNOTS('',3,(#18624,#18625,#18626,#18627,#18628,
#18629,#18630,#18631,#18632,#18633,#18634,#18635,#18636,#18637,#18638,#18639,
#18640,#18641,#18642,#18643,#18644,#18645),.UNSPECIFIED.,.F.,.F.,(4,3,3,
3,3,3,3,4),(13.8759337553363,14.627209984645,15.6023573169546,16.5775046492643,
17.552651981574,18.5277993138836,19.5029466461933,20.1591190625159),
 .UNSPECIFIED.);
#517=B_SPLINE_CURVE_WITH_KNOTS('',3,(#18646,#18647,#18648,#18649,#18650,
#18651,#18652,#18653,#18654,#18655,#18656,#18657,#18658,#18659,#18660,#18661,
#18662,#18663,#18664,#18665,#18666,#18667),.UNSPECIFIED.,.F.,.F.,(4,3,3,
3,3,3,3,4),(-16.4189726187288,-15.6023573169546,-14.627209984645,-13.6520626523353,
-12.6769153200256,-11.701767987716,-10.7266206554063,-10.1357873115492),
 .UNSPECIFIED.);
#518=B_SPLINE_CURVE_WITH_KNOTS('',3,(#18673,#18674,#18675,#18676,#18677,
#18678,#18679,#18680,#18681,#18682,#18683,#18684,#18685),.UNSPECIFIED.,
 .F.,.F.,(4,3,3,3,4),(-3.8526020043696,-2.92544199692899,-1.95029466461933,
-0.975147332309664,0.),.UNSPECIFIED.);
#519=B_SPLINE_CURVE_WITH_KNOTS('',3,(#18688,#18689,#18690,#18691,#18692,
#18693,#18694,#18695,#18696,#18697,#18698,#18699,#18700,#18701,#18702,#18703,
#18704,#18705,#18706),.UNSPECIFIED.,.F.,.F.,(4,3,3,3,3,3,4),(2.02057249175693,
2.925441996929,3.90058932923866,4.87573666154832,5.85088399385799,6.82603132616766,
7.59274844815668),.UNSPECIFIED.);
#520=B_SPLINE_CURVE_WITH_KNOTS('',3,(#18712,#18713,#18714,#18715,#18716,
#18717,#18718),.UNSPECIFIED.,.F.,.F.,(4,1,1,1,4),(40.8407044966673,41.1097812328693,
42.084928565179,43.0600758974886,44.0352232297983),.UNSPECIFIED.);
#521=B_SPLINE_CURVE_WITH_KNOTS('',3,(#18721,#18722,#18723,#18724,#18725,
#18726,#18727),.UNSPECIFIED.,.F.,.F.,(4,1,1,1,4),(40.8407044966673,41.7025254316425,
42.6776727639522,43.6528200962618,44.5576896014339),.UNSPECIFIED.);
#522=B_SPLINE_CURVE_WITH_KNOTS('',3,(#18732,#18733,#18734,#18735,#18736,
#18737,#18738,#18739,#18740,#18741),.UNSPECIFIED.,.F.,.F.,(4,1,1,1,1,1,
1,4),(34.5575191894877,35.2588972390113,36.234044571321,37.2091919036307,
38.1843392359403,39.15948656825,40.1346339005596,40.8407044966673),
 .UNSPECIFIED.);
#523=B_SPLINE_CURVE_WITH_KNOTS('',3,(#18742,#18743,#18744,#18745,#18746,
#18747,#18748,#18749,#18750,#18751,#18752),.UNSPECIFIED.,.F.,.F.,(4,1,1,
1,1,1,1,1,4),(34.5575191894877,34.8764941054748,35.8516414377845,36.8267887700942,
37.8019361024038,38.7770834347135,39.7522307670232,40.7273780993328,40.8407044966673),
 .UNSPECIFIED.);
#524=B_SPLINE_CURVE_WITH_KNOTS('',3,(#18757,#18758,#18759,#18760,#18761,
#18762,#18763,#18764,#18765,#18766,#18767),.UNSPECIFIED.,.F.,.F.,(4,1,1,
1,1,1,1,1,4),(28.2743338823081,28.4328659128437,29.4080132451533,30.383160577463,
31.3583079097727,32.3334552420823,33.308602574392,34.2837499067017,34.5575191894877),
 .UNSPECIFIED.);
#525=B_SPLINE_CURVE_WITH_KNOTS('',3,(#18768,#18769,#18770,#18771,#18772,
#18773,#18774,#18775,#18776,#18777),.UNSPECIFIED.,.F.,.F.,(4,1,1,1,1,1,
1,4),(28.2743338823081,29.0256101116168,30.0007574439265,30.9759047762362,
31.9510521085458,32.9261994408555,33.9013467731652,34.5575191894877),
 .UNSPECIFIED.);
#526=B_SPLINE_CURVE_WITH_KNOTS('',3,(#18782,#18783,#18784,#18785,#18786,
#18787,#18788,#18789,#18790,#18791),.UNSPECIFIED.,.F.,.F.,(4,1,1,1,1,1,
1,4),(21.9911485751285,22.5819819189857,23.5571292512954,24.532276583605,
25.5074239159147,26.4825712482243,27.457718580534,28.2743338823081),
 .UNSPECIFIED.);
#527=B_SPLINE_CURVE_WITH_KNOTS('',3,(#18792,#18793,#18794,#18795,#18796,
#18797,#18798,#18799,#18800,#18801,#18802),.UNSPECIFIED.,.F.,.F.,(4,1,1,
1,1,1,1,1,4),(21.9911485751285,22.1995787854492,23.1747261177589,24.1498734500685,
25.1250207823782,26.1001681146879,27.0753154469975,28.0504627793072,28.2743338823081),
 .UNSPECIFIED.);
#528=B_SPLINE_CURVE_WITH_KNOTS('',3,(#18808,#18809,#18810,#18811,#18812),
 .UNSPECIFIED.,.F.,.F.,(4,1,4),(14.3984001269719,15.3735474592815,15.7079632679489),
 .UNSPECIFIED.);
#529=B_SPLINE_CURVE_WITH_KNOTS('',3,(#18815,#18816,#18817,#18818,#18819),
 .UNSPECIFIED.,.F.,.F.,(4,1,4),(13.8759337553363,14.7808032605084,15.7079632679489),
 .UNSPECIFIED.);
#530=B_SPLINE_CURVE_WITH_KNOTS('',3,(#18821,#18822,#18823,#18824,#18825,
#18826,#18827,#18828,#18829,#18830,#18831),.UNSPECIFIED.,.F.,.F.,(4,1,1,
1,1,1,1,1,4),(15.7079632679489,15.755950592818,16.7310979251277,17.7062452574374,
18.681392589747,19.6565399220567,20.6316872543664,21.606834586676,21.9911485751285),
 .UNSPECIFIED.);
#531=B_SPLINE_CURVE_WITH_KNOTS('',3,(#18832,#18833,#18834,#18835,#18836,
#18837,#18838,#18839,#18840,#18841),.UNSPECIFIED.,.F.,.F.,(4,1,1,1,1,1,
1,4),(15.7079632679489,16.3486947915912,17.3238421239009,18.2989894562105,
19.2741367885202,20.2492841208299,21.2244314531395,21.9911485751285),
 .UNSPECIFIED.);
#532=B_SPLINE_CURVE_WITH_KNOTS('',3,(#18986,#18987,#18988,#18989,#18990,
#18991,#18992,#18993,#18994,#18995,#18996,#18997,#18998,#18999,#19000,#19001,
#19002,#19003,#19004,#19005,#19006,#19007,#19008,#19009,#19010,#19011,#19012,
#19013,#19014,#19015,#19016,#19017,#19018,#19019,#19020,#19021,#19022,#19023,
#19024,#19025,#19026,#19027,#19028,#19029,#19030,#19031,#19032,#19033,#19034),
 .UNSPECIFIED.,.F.,.F.,(4,3,3,3,3,3,3,3,3,3,3,3,3,3,3,3,4),(0.,0.0320333804888866,
0.0505515708593653,0.0603413132804416,0.0917900141854983,0.108096115778005,
0.122914675479851,0.145143248337739,0.168151513577436,0.177516949333476,
0.202471322707608,0.21794283081622,0.231200110368267,0.247503117401854,
0.263651632124391,0.277334442830003,0.286347380332244),.UNSPECIFIED.);
#533=B_SPLINE_CURVE_WITH_KNOTS('',3,(#19035,#19036,#19037,#19038,#19039,
#19040,#19041,#19042,#19043,#19044,#19045,#19046,#19047,#19048,#19049,#19050,
#19051,#19052,#19053,#19054,#19055,#19056,#19057,#19058,#19059,#19060,#19061,
#19062,#19063,#19064,#19065,#19066,#19067,#19068,#19069,#19070,#19071,#19072,
#19073,#19074,#19075,#19076,#19077,#19078,#19079,#19080,#19081,#19082,#19083),
 .UNSPECIFIED.,.F.,.F.,(4,3,3,3,3,3,3,3,3,3,3,3,3,3,3,3,4),(0.,0.0274305464075637,
0.0492901149097146,0.0591933555873536,0.0887250095166089,0.100015570674795,
0.108381796308415,0.130826479038955,0.152531076563578,0.162815893631175,
0.190691958353668,0.212372986031639,0.222945305605857,0.245534254906135,
0.257847836118801,0.274320152521146,0.28514280399515),.UNSPECIFIED.);
#534=B_SPLINE_CURVE_WITH_KNOTS('',3,(#19084,#19085,#19086,#19087,#19088,
#19089,#19090,#19091,#19092,#19093,#19094,#19095,#19096,#19097,#19098,#19099,
#19100,#19101,#19102,#19103,#19104,#19105,#19106,#19107,#19108),
 .UNSPECIFIED.,.F.,.F.,(4,3,3,3,3,3,3,3,4),(-10.1357873115492,-9.75147332309665,
-8.77632599078699,-7.80117865847732,-6.82603132616766,-5.85088399385799,
-4.87573666154833,-3.90058932923866,-3.8526020043696),.UNSPECIFIED.);
#535=B_SPLINE_CURVE_WITH_KNOTS('',3,(#19253,#19254,#19255,#19256,#19257,
#19258,#19259,#19260,#19261,#19262,#19263,#19264,#19265,#19266,#19267,#19268,
#19269,#19270,#19271,#19272,#19273,#19274,#19275,#19276,#19277,#19278,#19279,
#19280,#19281,#19282,#19283,#19284,#19285,#19286,#19287,#19288,#19289,#19290,
#19291,#19292,#19293,#19294,#19295,#19296,#19297,#19298,#19299,#19300,#19301),
 .UNSPECIFIED.,.F.,.F.,(4,3,3,3,3,3,3,3,3,3,3,3,3,3,3,3,4),(0.,0.0274305890506951,
0.0492901290331875,0.0591933603491513,0.0887250177779717,0.100015607166709,
0.108381835831352,0.13082647903896,0.152531071764912,0.162815892251191,
0.190691957318683,0.212372984486691,0.22294529735758,0.245534140364172,
0.257847701250626,0.274320152521159,0.285142803995162),.UNSPECIFIED.);
#536=B_SPLINE_CURVE_WITH_KNOTS('',3,(#19302,#19303,#19304,#19305,#19306,
#19307,#19308,#19309,#19310,#19311,#19312,#19313,#19314,#19315,#19316,#19317,
#19318,#19319,#19320,#19321,#19322,#19323,#19324,#19325,#19326),
 .UNSPECIFIED.,.F.,.F.,(4,3,3,3,3,3,3,3,4),(7.59274844815668,7.80117865847732,
8.77632599078698,9.75147332309665,10.7266206554063,11.701767987716,12.6769153200256,
13.6520626523353,13.8759337553363),.UNSPECIFIED.);
#537=B_SPLINE_CURVE_WITH_KNOTS('',3,(#19327,#19328,#19329,#19330,#19331,
#19332,#19333,#19334,#19335,#19336,#19337,#19338,#19339,#19340,#19341,#19342,
#19343,#19344,#19345,#19346,#19347,#19348,#19349,#19350,#19351,#19352,#19353,
#19354,#19355,#19356,#19357,#19358,#19359,#19360,#19361,#19362,#19363,#19364,
#19365,#19366,#19367,#19368,#19369,#19370,#19371,#19372,#19373,#19374,#19375),
 .UNSPECIFIED.,.F.,.F.,(4,3,3,3,3,3,3,3,3,3,3,3,3,3,3,3,4),(0.,0.0320334058164849,
0.0505515938322513,0.0603413311462071,0.0917900214840119,0.108096111687201,
0.122914678304232,0.145143248337743,0.168151527562726,0.177516955081398,
0.202471327018552,0.217942288122009,0.231200024743484,0.24750284136614,
0.263651600306541,0.277334442830014,0.286347380332252),.UNSPECIFIED.);
#538=SHAPE_REPRESENTATION_RELATIONSHIP('SRR','None',#19517,#548);
#539=SHAPE_REPRESENTATION_RELATIONSHIP('SRR','None',#19518,#549);
#540=SHAPE_REPRESENTATION_RELATIONSHIP('SRR','None',#19519,#550);
#541=SHAPE_REPRESENTATION_RELATIONSHIP('SRR','None',#19520,#551);
#542=SHAPE_REPRESENTATION_RELATIONSHIP('SRR','None',#19522,#552);
#543=SHAPE_REPRESENTATION_RELATIONSHIP('SRR','None',#19523,#553);
#544=SHAPE_REPRESENTATION_RELATIONSHIP('SRR','None',#19524,#554);
#545=SHAPE_REPRESENTATION_RELATIONSHIP('SRR','None',#19525,#555);
#546=SHAPE_REPRESENTATION_RELATIONSHIP('SRR','None',#19526,#556);
#547=SHAPE_REPRESENTATION_RELATIONSHIP('SRR','None',#19527,#557);
#548=ADVANCED_BREP_SHAPE_REPRESENTATION('',(#568),#19460);
#549=ADVANCED_BREP_SHAPE_REPRESENTATION('',(#569),#19461);
#550=ADVANCED_BREP_SHAPE_REPRESENTATION('',(#570),#19462);
#551=ADVANCED_BREP_SHAPE_REPRESENTATION('',(#571),#19463);
#552=ADVANCED_BREP_SHAPE_REPRESENTATION('',(#572),#19465);
#553=ADVANCED_BREP_SHAPE_REPRESENTATION('',(#573),#19466);
#554=ADVANCED_BREP_SHAPE_REPRESENTATION('',(#574),#19467);
#555=ADVANCED_BREP_SHAPE_REPRESENTATION('',(#575),#19468);
#556=ADVANCED_BREP_SHAPE_REPRESENTATION('',(#576),#19469);
#557=ADVANCED_BREP_SHAPE_REPRESENTATION('',(#577),#19470);
#558=STYLED_ITEM('',(#19581),#568);
#559=STYLED_ITEM('',(#19581),#569);
#560=STYLED_ITEM('',(#19582),#570);
#561=STYLED_ITEM('',(#19583),#571);
#562=STYLED_ITEM('',(#19584),#572);
#563=STYLED_ITEM('',(#19584),#573);
#564=STYLED_ITEM('',(#19585),#574);
#565=STYLED_ITEM('',(#19583),#575);
#566=STYLED_ITEM('',(#19586),#576);
#567=STYLED_ITEM('',(#19587),#577);
#568=MANIFOLD_SOLID_BREP('Body1',#7151);
#569=MANIFOLD_SOLID_BREP('Body1',#7152);
#570=MANIFOLD_SOLID_BREP('Body1',#7153);
#571=MANIFOLD_SOLID_BREP('Body1',#7154);
#572=MANIFOLD_SOLID_BREP('Body1',#7155);
#573=MANIFOLD_SOLID_BREP('Body1',#7156);
#574=MANIFOLD_SOLID_BREP('Body1',#7157);
#575=MANIFOLD_SOLID_BREP('Body1',#7158);
#576=MANIFOLD_SOLID_BREP('Body1',#7159);
#577=MANIFOLD_SOLID_BREP('Body1',#7160);
#578=TOROIDAL_SURFACE('',#7315,1.2,0.1);
#579=TOROIDAL_SURFACE('',#7321,1.2,0.1);
#580=TOROIDAL_SURFACE('',#7375,1.2,0.1);
#581=TOROIDAL_SURFACE('',#7381,1.2,0.1);
#582=FACE_BOUND('',#1246,.T.);
#583=FACE_BOUND('',#1247,.T.);
#584=FACE_BOUND('',#1248,.T.);
#585=FACE_BOUND('',#1249,.T.);
#586=FACE_BOUND('',#1254,.T.);
#587=FACE_BOUND('',#1255,.T.);
#588=FACE_BOUND('',#1256,.T.);
#589=FACE_BOUND('',#1257,.T.);
#590=FACE_BOUND('',#1286,.T.);
#591=FACE_BOUND('',#1287,.T.);
#592=FACE_BOUND('',#1288,.T.);
#593=FACE_BOUND('',#1289,.T.);
#594=FACE_BOUND('',#1296,.T.);
#595=FACE_BOUND('',#1297,.T.);
#596=FACE_BOUND('',#1298,.T.);
#597=FACE_BOUND('',#1299,.T.);
#598=FACE_BOUND('',#1315,.T.);
#599=FACE_BOUND('',#1317,.T.);
#600=FACE_BOUND('',#1320,.T.);
#601=FACE_BOUND('',#1337,.T.);
#602=FACE_BOUND('',#1340,.T.);
#603=FACE_BOUND('',#1351,.T.);
#604=FACE_BOUND('',#1353,.T.);
#605=FACE_BOUND('',#1365,.T.);
#606=FACE_BOUND('',#1374,.T.);
#607=FACE_BOUND('',#1375,.T.);
#608=FACE_BOUND('',#1376,.T.);
#609=FACE_BOUND('',#1391,.T.);
#610=FACE_BOUND('',#1392,.T.);
#611=FACE_BOUND('',#1393,.T.);
#612=FACE_BOUND('',#1429,.T.);
#613=FACE_BOUND('',#1430,.T.);
#614=FACE_BOUND('',#1431,.T.);
#615=FACE_BOUND('',#1432,.T.);
#616=FACE_BOUND('',#1433,.T.);
#617=FACE_BOUND('',#1434,.T.);
#618=FACE_BOUND('',#1448,.T.);
#619=FACE_BOUND('',#1456,.T.);
#620=FACE_BOUND('',#1467,.T.);
#621=FACE_BOUND('',#1469,.T.);
#622=FACE_BOUND('',#1481,.T.);
#623=FACE_BOUND('',#1490,.T.);
#624=FACE_BOUND('',#1491,.T.);
#625=FACE_BOUND('',#1492,.T.);
#626=FACE_BOUND('',#1507,.T.);
#627=FACE_BOUND('',#1508,.T.);
#628=FACE_BOUND('',#1509,.T.);
#629=FACE_BOUND('',#1545,.T.);
#630=FACE_BOUND('',#1546,.T.);
#631=FACE_BOUND('',#1547,.T.);
#632=FACE_BOUND('',#1548,.T.);
#633=FACE_BOUND('',#1549,.T.);
#634=FACE_BOUND('',#1550,.T.);
#635=FACE_BOUND('',#1556,.T.);
#636=FACE_BOUND('',#1560,.T.);
#637=FACE_BOUND('',#1564,.T.);
#638=FACE_BOUND('',#1568,.T.);
#639=FACE_BOUND('',#1588,.T.);
#640=FACE_BOUND('',#1589,.T.);
#641=FACE_BOUND('',#1594,.T.);
#642=FACE_BOUND('',#1595,.T.);
#643=FACE_BOUND('',#1596,.T.);
#644=FACE_BOUND('',#1597,.T.);
#645=FACE_BOUND('',#1598,.T.);
#646=FACE_BOUND('',#1599,.T.);
#647=FACE_BOUND('',#1674,.T.);
#648=FACE_BOUND('',#1677,.T.);
#649=FACE_BOUND('',#1693,.T.);
#650=FACE_BOUND('',#1702,.T.);
#651=FACE_BOUND('',#1706,.T.);
#652=FACE_BOUND('',#1708,.T.);
#653=PLANE('',#7283);
#654=PLANE('',#7284);
#655=PLANE('',#7285);
#656=PLANE('',#7286);
#657=PLANE('',#7288);
#658=PLANE('',#7294);
#659=PLANE('',#7295);
#660=PLANE('',#7296);
#661=PLANE('',#7297);
#662=PLANE('',#7298);
#663=PLANE('',#7299);
#664=PLANE('',#7300);
#665=PLANE('',#7306);
#666=PLANE('',#7311);
#667=PLANE('',#7325);
#668=PLANE('',#7326);
#669=PLANE('',#7327);
#670=PLANE('',#7328);
#671=PLANE('',#7329);
#672=PLANE('',#7330);
#673=PLANE('',#7331);
#674=PLANE('',#7332);
#675=PLANE('',#7343);
#676=PLANE('',#7344);
#677=PLANE('',#7345);
#678=PLANE('',#7346);
#679=PLANE('',#7348);
#680=PLANE('',#7350);
#681=PLANE('',#7355);
#682=PLANE('',#7356);
#683=PLANE('',#7357);
#684=PLANE('',#7358);
#685=PLANE('',#7364);
#686=PLANE('',#7365);
#687=PLANE('',#7366);
#688=PLANE('',#7371);
#689=PLANE('',#7385);
#690=PLANE('',#7386);
#691=PLANE('',#7387);
#692=PLANE('',#7388);
#693=PLANE('',#7389);
#694=PLANE('',#7390);
#695=PLANE('',#7391);
#696=PLANE('',#7392);
#697=PLANE('',#7397);
#698=PLANE('',#7399);
#699=PLANE('',#7403);
#700=PLANE('',#7408);
#701=PLANE('',#7410);
#702=PLANE('',#7412);
#703=PLANE('',#7413);
#704=PLANE('',#7414);
#705=PLANE('',#7421);
#706=PLANE('',#7439);
#707=PLANE('',#7444);
#708=PLANE('',#7450);
#709=PLANE('',#7451);
#710=PLANE('',#7452);
#711=PLANE('',#7453);
#712=PLANE('',#7454);
#713=PLANE('',#7455);
#714=PLANE('',#7456);
#715=PLANE('',#7457);
#716=PLANE('',#7459);
#717=PLANE('',#7461);
#718=PLANE('',#7462);
#719=PLANE('',#7463);
#720=PLANE('',#7464);
#721=PLANE('',#7465);
#722=PLANE('',#7466);
#723=PLANE('',#7467);
#724=PLANE('',#7468);
#725=PLANE('',#7469);
#726=PLANE('',#7470);
#727=PLANE('',#7471);
#728=PLANE('',#7476);
#729=PLANE('',#7478);
#730=PLANE('',#7479);
#731=PLANE('',#7480);
#732=PLANE('',#7481);
#733=PLANE('',#7482);
#734=PLANE('',#7483);
#735=PLANE('',#7484);
#736=PLANE('',#7486);
#737=PLANE('',#7503);
#738=PLANE('',#7522);
#739=PLANE('',#7523);
#740=PLANE('',#7524);
#741=PLANE('',#7538);
#742=PLANE('',#7539);
#743=PLANE('',#7540);
#744=PLANE('',#7541);
#745=PLANE('',#7542);
#746=PLANE('',#7543);
#747=PLANE('',#7544);
#748=PLANE('',#7546);
#749=PLANE('',#7547);
#750=PLANE('',#7548);
#751=PLANE('',#7549);
#752=PLANE('',#7550);
#753=PLANE('',#7551);
#754=PLANE('',#7552);
#755=PLANE('',#7558);
#756=PLANE('',#7559);
#757=PLANE('',#7560);
#758=PLANE('',#7561);
#759=PLANE('',#7562);
#760=PLANE('',#7563);
#761=PLANE('',#7564);
#762=PLANE('',#7565);
#763=PLANE('',#7567);
#764=PLANE('',#7569);
#765=PLANE('',#7570);
#766=PLANE('',#7571);
#767=PLANE('',#7572);
#768=PLANE('',#7573);
#769=PLANE('',#7574);
#770=PLANE('',#7575);
#771=PLANE('',#7576);
#772=PLANE('',#7577);
#773=PLANE('',#7578);
#774=PLANE('',#7579);
#775=PLANE('',#7584);
#776=PLANE('',#7586);
#777=PLANE('',#7587);
#778=PLANE('',#7588);
#779=PLANE('',#7589);
#780=PLANE('',#7590);
#781=PLANE('',#7591);
#782=PLANE('',#7592);
#783=PLANE('',#7594);
#784=PLANE('',#7611);
#785=PLANE('',#7630);
#786=PLANE('',#7631);
#787=PLANE('',#7632);
#788=PLANE('',#7640);
#789=PLANE('',#7645);
#790=PLANE('',#7646);
#791=PLANE('',#7651);
#792=PLANE('',#7652);
#793=PLANE('',#7657);
#794=PLANE('',#7658);
#795=PLANE('',#7663);
#796=PLANE('',#7682);
#797=PLANE('',#7683);
#798=PLANE('',#7684);
#799=PLANE('',#7685);
#800=PLANE('',#7755);
#801=PLANE('',#7756);
#802=PLANE('',#7757);
#803=PLANE('',#7758);
#804=PLANE('',#7759);
#805=PLANE('',#7760);
#806=PLANE('',#7761);
#807=PLANE('',#7762);
#808=PLANE('',#7766);
#809=PLANE('',#7767);
#810=PLANE('',#7785);
#811=PLANE('',#7787);
#812=PLANE('',#7788);
#813=PLANE('',#7789);
#814=PLANE('',#7790);
#815=PLANE('',#7791);
#816=PLANE('',#7792);
#817=PLANE('',#7793);
#818=PLANE('',#7809);
#819=PLANE('',#7810);
#820=FACE_OUTER_BOUND('',#1229,.T.);
#821=FACE_OUTER_BOUND('',#1230,.T.);
#822=FACE_OUTER_BOUND('',#1231,.T.);
#823=FACE_OUTER_BOUND('',#1232,.T.);
#824=FACE_OUTER_BOUND('',#1233,.T.);
#825=FACE_OUTER_BOUND('',#1234,.T.);
#826=FACE_OUTER_BOUND('',#1235,.T.);
#827=FACE_OUTER_BOUND('',#1236,.T.);
#828=FACE_OUTER_BOUND('',#1237,.T.);
#829=FACE_OUTER_BOUND('',#1238,.T.);
#830=FACE_OUTER_BOUND('',#1239,.T.);
#831=FACE_OUTER_BOUND('',#1240,.T.);
#832=FACE_OUTER_BOUND('',#1241,.T.);
#833=FACE_OUTER_BOUND('',#1242,.T.);
#834=FACE_OUTER_BOUND('',#1243,.T.);
#835=FACE_OUTER_BOUND('',#1244,.T.);
#836=FACE_OUTER_BOUND('',#1245,.T.);
#837=FACE_OUTER_BOUND('',#1250,.T.);
#838=FACE_OUTER_BOUND('',#1251,.T.);
#839=FACE_OUTER_BOUND('',#1252,.T.);
#840=FACE_OUTER_BOUND('',#1253,.T.);
#841=FACE_OUTER_BOUND('',#1258,.T.);
#842=FACE_OUTER_BOUND('',#1259,.T.);
#843=FACE_OUTER_BOUND('',#1260,.T.);
#844=FACE_OUTER_BOUND('',#1261,.T.);
#845=FACE_OUTER_BOUND('',#1262,.T.);
#846=FACE_OUTER_BOUND('',#1263,.T.);
#847=FACE_OUTER_BOUND('',#1264,.T.);
#848=FACE_OUTER_BOUND('',#1265,.T.);
#849=FACE_OUTER_BOUND('',#1266,.T.);
#850=FACE_OUTER_BOUND('',#1267,.T.);
#851=FACE_OUTER_BOUND('',#1268,.T.);
#852=FACE_OUTER_BOUND('',#1269,.T.);
#853=FACE_OUTER_BOUND('',#1270,.T.);
#854=FACE_OUTER_BOUND('',#1271,.T.);
#855=FACE_OUTER_BOUND('',#1272,.T.);
#856=FACE_OUTER_BOUND('',#1273,.T.);
#857=FACE_OUTER_BOUND('',#1274,.T.);
#858=FACE_OUTER_BOUND('',#1275,.T.);
#859=FACE_OUTER_BOUND('',#1276,.T.);
#860=FACE_OUTER_BOUND('',#1277,.T.);
#861=FACE_OUTER_BOUND('',#1278,.T.);
#862=FACE_OUTER_BOUND('',#1279,.T.);
#863=FACE_OUTER_BOUND('',#1280,.T.);
#864=FACE_OUTER_BOUND('',#1281,.T.);
#865=FACE_OUTER_BOUND('',#1282,.T.);
#866=FACE_OUTER_BOUND('',#1283,.T.);
#867=FACE_OUTER_BOUND('',#1284,.T.);
#868=FACE_OUTER_BOUND('',#1285,.T.);
#869=FACE_OUTER_BOUND('',#1290,.T.);
#870=FACE_OUTER_BOUND('',#1291,.T.);
#871=FACE_OUTER_BOUND('',#1292,.T.);
#872=FACE_OUTER_BOUND('',#1293,.T.);
#873=FACE_OUTER_BOUND('',#1294,.T.);
#874=FACE_OUTER_BOUND('',#1295,.T.);
#875=FACE_OUTER_BOUND('',#1300,.T.);
#876=FACE_OUTER_BOUND('',#1301,.T.);
#877=FACE_OUTER_BOUND('',#1302,.T.);
#878=FACE_OUTER_BOUND('',#1303,.T.);
#879=FACE_OUTER_BOUND('',#1304,.T.);
#880=FACE_OUTER_BOUND('',#1305,.T.);
#881=FACE_OUTER_BOUND('',#1306,.T.);
#882=FACE_OUTER_BOUND('',#1307,.T.);
#883=FACE_OUTER_BOUND('',#1308,.T.);
#884=FACE_OUTER_BOUND('',#1309,.T.);
#885=FACE_OUTER_BOUND('',#1310,.T.);
#886=FACE_OUTER_BOUND('',#1311,.T.);
#887=FACE_OUTER_BOUND('',#1312,.T.);
#888=FACE_OUTER_BOUND('',#1313,.T.);
#889=FACE_OUTER_BOUND('',#1314,.T.);
#890=FACE_OUTER_BOUND('',#1316,.T.);
#891=FACE_OUTER_BOUND('',#1318,.T.);
#892=FACE_OUTER_BOUND('',#1319,.T.);
#893=FACE_OUTER_BOUND('',#1321,.T.);
#894=FACE_OUTER_BOUND('',#1322,.T.);
#895=FACE_OUTER_BOUND('',#1323,.T.);
#896=FACE_OUTER_BOUND('',#1324,.T.);
#897=FACE_OUTER_BOUND('',#1325,.T.);
#898=FACE_OUTER_BOUND('',#1326,.T.);
#899=FACE_OUTER_BOUND('',#1327,.T.);
#900=FACE_OUTER_BOUND('',#1328,.T.);
#901=FACE_OUTER_BOUND('',#1329,.T.);
#902=FACE_OUTER_BOUND('',#1330,.T.);
#903=FACE_OUTER_BOUND('',#1331,.T.);
#904=FACE_OUTER_BOUND('',#1332,.T.);
#905=FACE_OUTER_BOUND('',#1333,.T.);
#906=FACE_OUTER_BOUND('',#1334,.T.);
#907=FACE_OUTER_BOUND('',#1335,.T.);
#908=FACE_OUTER_BOUND('',#1336,.T.);
#909=FACE_OUTER_BOUND('',#1338,.T.);
#910=FACE_OUTER_BOUND('',#1339,.T.);
#911=FACE_OUTER_BOUND('',#1341,.T.);
#912=FACE_OUTER_BOUND('',#1342,.T.);
#913=FACE_OUTER_BOUND('',#1343,.T.);
#914=FACE_OUTER_BOUND('',#1344,.T.);
#915=FACE_OUTER_BOUND('',#1345,.T.);
#916=FACE_OUTER_BOUND('',#1346,.T.);
#917=FACE_OUTER_BOUND('',#1347,.T.);
#918=FACE_OUTER_BOUND('',#1348,.T.);
#919=FACE_OUTER_BOUND('',#1349,.T.);
#920=FACE_OUTER_BOUND('',#1350,.T.);
#921=FACE_OUTER_BOUND('',#1352,.T.);
#922=FACE_OUTER_BOUND('',#1354,.T.);
#923=FACE_OUTER_BOUND('',#1355,.T.);
#924=FACE_OUTER_BOUND('',#1356,.T.);
#925=FACE_OUTER_BOUND('',#1357,.T.);
#926=FACE_OUTER_BOUND('',#1358,.T.);
#927=FACE_OUTER_BOUND('',#1359,.T.);
#928=FACE_OUTER_BOUND('',#1360,.T.);
#929=FACE_OUTER_BOUND('',#1361,.T.);
#930=FACE_OUTER_BOUND('',#1362,.T.);
#931=FACE_OUTER_BOUND('',#1363,.T.);
#932=FACE_OUTER_BOUND('',#1364,.T.);
#933=FACE_OUTER_BOUND('',#1366,.T.);
#934=FACE_OUTER_BOUND('',#1367,.T.);
#935=FACE_OUTER_BOUND('',#1368,.T.);
#936=FACE_OUTER_BOUND('',#1369,.T.);
#937=FACE_OUTER_BOUND('',#1370,.T.);
#938=FACE_OUTER_BOUND('',#1371,.T.);
#939=FACE_OUTER_BOUND('',#1372,.T.);
#940=FACE_OUTER_BOUND('',#1373,.T.);
#941=FACE_OUTER_BOUND('',#1377,.T.);
#942=FACE_OUTER_BOUND('',#1378,.T.);
#943=FACE_OUTER_BOUND('',#1379,.T.);
#944=FACE_OUTER_BOUND('',#1380,.T.);
#945=FACE_OUTER_BOUND('',#1381,.T.);
#946=FACE_OUTER_BOUND('',#1382,.T.);
#947=FACE_OUTER_BOUND('',#1383,.T.);
#948=FACE_OUTER_BOUND('',#1384,.T.);
#949=FACE_OUTER_BOUND('',#1385,.T.);
#950=FACE_OUTER_BOUND('',#1386,.T.);
#951=FACE_OUTER_BOUND('',#1387,.T.);
#952=FACE_OUTER_BOUND('',#1388,.T.);
#953=FACE_OUTER_BOUND('',#1389,.T.);
#954=FACE_OUTER_BOUND('',#1390,.T.);
#955=FACE_OUTER_BOUND('',#1394,.T.);
#956=FACE_OUTER_BOUND('',#1395,.T.);
#957=FACE_OUTER_BOUND('',#1396,.T.);
#958=FACE_OUTER_BOUND('',#1397,.T.);
#959=FACE_OUTER_BOUND('',#1398,.T.);
#960=FACE_OUTER_BOUND('',#1399,.T.);
#961=FACE_OUTER_BOUND('',#1400,.T.);
#962=FACE_OUTER_BOUND('',#1401,.T.);
#963=FACE_OUTER_BOUND('',#1402,.T.);
#964=FACE_OUTER_BOUND('',#1403,.T.);
#965=FACE_OUTER_BOUND('',#1404,.T.);
#966=FACE_OUTER_BOUND('',#1405,.T.);
#967=FACE_OUTER_BOUND('',#1406,.T.);
#968=FACE_OUTER_BOUND('',#1407,.T.);
#969=FACE_OUTER_BOUND('',#1408,.T.);
#970=FACE_OUTER_BOUND('',#1409,.T.);
#971=FACE_OUTER_BOUND('',#1410,.T.);
#972=FACE_OUTER_BOUND('',#1411,.T.);
#973=FACE_OUTER_BOUND('',#1412,.T.);
#974=FACE_OUTER_BOUND('',#1413,.T.);
#975=FACE_OUTER_BOUND('',#1414,.T.);
#976=FACE_OUTER_BOUND('',#1415,.T.);
#977=FACE_OUTER_BOUND('',#1416,.T.);
#978=FACE_OUTER_BOUND('',#1417,.T.);
#979=FACE_OUTER_BOUND('',#1418,.T.);
#980=FACE_OUTER_BOUND('',#1419,.T.);
#981=FACE_OUTER_BOUND('',#1420,.T.);
#982=FACE_OUTER_BOUND('',#1421,.T.);
#983=FACE_OUTER_BOUND('',#1422,.T.);
#984=FACE_OUTER_BOUND('',#1423,.T.);
#985=FACE_OUTER_BOUND('',#1424,.T.);
#986=FACE_OUTER_BOUND('',#1425,.T.);
#987=FACE_OUTER_BOUND('',#1426,.T.);
#988=FACE_OUTER_BOUND('',#1427,.T.);
#989=FACE_OUTER_BOUND('',#1428,.T.);
#990=FACE_OUTER_BOUND('',#1435,.T.);
#991=FACE_OUTER_BOUND('',#1436,.T.);
#992=FACE_OUTER_BOUND('',#1437,.T.);
#993=FACE_OUTER_BOUND('',#1438,.T.);
#994=FACE_OUTER_BOUND('',#1439,.T.);
#995=FACE_OUTER_BOUND('',#1440,.T.);
#996=FACE_OUTER_BOUND('',#1441,.T.);
#997=FACE_OUTER_BOUND('',#1442,.T.);
#998=FACE_OUTER_BOUND('',#1443,.T.);
#999=FACE_OUTER_BOUND('',#1444,.T.);
#1000=FACE_OUTER_BOUND('',#1445,.T.);
#1001=FACE_OUTER_BOUND('',#1446,.T.);
#1002=FACE_OUTER_BOUND('',#1447,.T.);
#1003=FACE_OUTER_BOUND('',#1449,.T.);
#1004=FACE_OUTER_BOUND('',#1450,.T.);
#1005=FACE_OUTER_BOUND('',#1451,.T.);
#1006=FACE_OUTER_BOUND('',#1452,.T.);
#1007=FACE_OUTER_BOUND('',#1453,.T.);
#1008=FACE_OUTER_BOUND('',#1454,.T.);
#1009=FACE_OUTER_BOUND('',#1455,.T.);
#1010=FACE_OUTER_BOUND('',#1457,.T.);
#1011=FACE_OUTER_BOUND('',#1458,.T.);
#1012=FACE_OUTER_BOUND('',#1459,.T.);
#1013=FACE_OUTER_BOUND('',#1460,.T.);
#1014=FACE_OUTER_BOUND('',#1461,.T.);
#1015=FACE_OUTER_BOUND('',#1462,.T.);
#1016=FACE_OUTER_BOUND('',#1463,.T.);
#1017=FACE_OUTER_BOUND('',#1464,.T.);
#1018=FACE_OUTER_BOUND('',#1465,.T.);
#1019=FACE_OUTER_BOUND('',#1466,.T.);
#1020=FACE_OUTER_BOUND('',#1468,.T.);
#1021=FACE_OUTER_BOUND('',#1470,.T.);
#1022=FACE_OUTER_BOUND('',#1471,.T.);
#1023=FACE_OUTER_BOUND('',#1472,.T.);
#1024=FACE_OUTER_BOUND('',#1473,.T.);
#1025=FACE_OUTER_BOUND('',#1474,.T.);
#1026=FACE_OUTER_BOUND('',#1475,.T.);
#1027=FACE_OUTER_BOUND('',#1476,.T.);
#1028=FACE_OUTER_BOUND('',#1477,.T.);
#1029=FACE_OUTER_BOUND('',#1478,.T.);
#1030=FACE_OUTER_BOUND('',#1479,.T.);
#1031=FACE_OUTER_BOUND('',#1480,.T.);
#1032=FACE_OUTER_BOUND('',#1482,.T.);
#1033=FACE_OUTER_BOUND('',#1483,.T.);
#1034=FACE_OUTER_BOUND('',#1484,.T.);
#1035=FACE_OUTER_BOUND('',#1485,.T.);
#1036=FACE_OUTER_BOUND('',#1486,.T.);
#1037=FACE_OUTER_BOUND('',#1487,.T.);
#1038=FACE_OUTER_BOUND('',#1488,.T.);
#1039=FACE_OUTER_BOUND('',#1489,.T.);
#1040=FACE_OUTER_BOUND('',#1493,.T.);
#1041=FACE_OUTER_BOUND('',#1494,.T.);
#1042=FACE_OUTER_BOUND('',#1495,.T.);
#1043=FACE_OUTER_BOUND('',#1496,.T.);
#1044=FACE_OUTER_BOUND('',#1497,.T.);
#1045=FACE_OUTER_BOUND('',#1498,.T.);
#1046=FACE_OUTER_BOUND('',#1499,.T.);
#1047=FACE_OUTER_BOUND('',#1500,.T.);
#1048=FACE_OUTER_BOUND('',#1501,.T.);
#1049=FACE_OUTER_BOUND('',#1502,.T.);
#1050=FACE_OUTER_BOUND('',#1503,.T.);
#1051=FACE_OUTER_BOUND('',#1504,.T.);
#1052=FACE_OUTER_BOUND('',#1505,.T.);
#1053=FACE_OUTER_BOUND('',#1506,.T.);
#1054=FACE_OUTER_BOUND('',#1510,.T.);
#1055=FACE_OUTER_BOUND('',#1511,.T.);
#1056=FACE_OUTER_BOUND('',#1512,.T.);
#1057=FACE_OUTER_BOUND('',#1513,.T.);
#1058=FACE_OUTER_BOUND('',#1514,.T.);
#1059=FACE_OUTER_BOUND('',#1515,.T.);
#1060=FACE_OUTER_BOUND('',#1516,.T.);
#1061=FACE_OUTER_BOUND('',#1517,.T.);
#1062=FACE_OUTER_BOUND('',#1518,.T.);
#1063=FACE_OUTER_BOUND('',#1519,.T.);
#1064=FACE_OUTER_BOUND('',#1520,.T.);
#1065=FACE_OUTER_BOUND('',#1521,.T.);
#1066=FACE_OUTER_BOUND('',#1522,.T.);
#1067=FACE_OUTER_BOUND('',#1523,.T.);
#1068=FACE_OUTER_BOUND('',#1524,.T.);
#1069=FACE_OUTER_BOUND('',#1525,.T.);
#1070=FACE_OUTER_BOUND('',#1526,.T.);
#1071=FACE_OUTER_BOUND('',#1527,.T.);
#1072=FACE_OUTER_BOUND('',#1528,.T.);
#1073=FACE_OUTER_BOUND('',#1529,.T.);
#1074=FACE_OUTER_BOUND('',#1530,.T.);
#1075=FACE_OUTER_BOUND('',#1531,.T.);
#1076=FACE_OUTER_BOUND('',#1532,.T.);
#1077=FACE_OUTER_BOUND('',#1533,.T.);
#1078=FACE_OUTER_BOUND('',#1534,.T.);
#1079=FACE_OUTER_BOUND('',#1535,.T.);
#1080=FACE_OUTER_BOUND('',#1536,.T.);
#1081=FACE_OUTER_BOUND('',#1537,.T.);
#1082=FACE_OUTER_BOUND('',#1538,.T.);
#1083=FACE_OUTER_BOUND('',#1539,.T.);
#1084=FACE_OUTER_BOUND('',#1540,.T.);
#1085=FACE_OUTER_BOUND('',#1541,.T.);
#1086=FACE_OUTER_BOUND('',#1542,.T.);
#1087=FACE_OUTER_BOUND('',#1543,.T.);
#1088=FACE_OUTER_BOUND('',#1544,.T.);
#1089=FACE_OUTER_BOUND('',#1551,.T.);
#1090=FACE_OUTER_BOUND('',#1552,.T.);
#1091=FACE_OUTER_BOUND('',#1553,.T.);
#1092=FACE_OUTER_BOUND('',#1554,.T.);
#1093=FACE_OUTER_BOUND('',#1555,.T.);
#1094=FACE_OUTER_BOUND('',#1557,.T.);
#1095=FACE_OUTER_BOUND('',#1558,.T.);
#1096=FACE_OUTER_BOUND('',#1559,.T.);
#1097=FACE_OUTER_BOUND('',#1561,.T.);
#1098=FACE_OUTER_BOUND('',#1562,.T.);
#1099=FACE_OUTER_BOUND('',#1563,.T.);
#1100=FACE_OUTER_BOUND('',#1565,.T.);
#1101=FACE_OUTER_BOUND('',#1566,.T.);
#1102=FACE_OUTER_BOUND('',#1567,.T.);
#1103=FACE_OUTER_BOUND('',#1569,.T.);
#1104=FACE_OUTER_BOUND('',#1570,.T.);
#1105=FACE_OUTER_BOUND('',#1571,.T.);
#1106=FACE_OUTER_BOUND('',#1572,.T.);
#1107=FACE_OUTER_BOUND('',#1573,.T.);
#1108=FACE_OUTER_BOUND('',#1574,.T.);
#1109=FACE_OUTER_BOUND('',#1575,.T.);
#1110=FACE_OUTER_BOUND('',#1576,.T.);
#1111=FACE_OUTER_BOUND('',#1577,.T.);
#1112=FACE_OUTER_BOUND('',#1578,.T.);
#1113=FACE_OUTER_BOUND('',#1579,.T.);
#1114=FACE_OUTER_BOUND('',#1580,.T.);
#1115=FACE_OUTER_BOUND('',#1581,.T.);
#1116=FACE_OUTER_BOUND('',#1582,.T.);
#1117=FACE_OUTER_BOUND('',#1583,.T.);
#1118=FACE_OUTER_BOUND('',#1584,.T.);
#1119=FACE_OUTER_BOUND('',#1585,.T.);
#1120=FACE_OUTER_BOUND('',#1586,.T.);
#1121=FACE_OUTER_BOUND('',#1587,.T.);
#1122=FACE_OUTER_BOUND('',#1590,.T.);
#1123=FACE_OUTER_BOUND('',#1591,.T.);
#1124=FACE_OUTER_BOUND('',#1592,.T.);
#1125=FACE_OUTER_BOUND('',#1593,.T.);
#1126=FACE_OUTER_BOUND('',#1600,.T.);
#1127=FACE_OUTER_BOUND('',#1601,.T.);
#1128=FACE_OUTER_BOUND('',#1602,.T.);
#1129=FACE_OUTER_BOUND('',#1603,.T.);
#1130=FACE_OUTER_BOUND('',#1604,.T.);
#1131=FACE_OUTER_BOUND('',#1605,.T.);
#1132=FACE_OUTER_BOUND('',#1606,.T.);
#1133=FACE_OUTER_BOUND('',#1607,.T.);
#1134=FACE_OUTER_BOUND('',#1608,.T.);
#1135=FACE_OUTER_BOUND('',#1609,.T.);
#1136=FACE_OUTER_BOUND('',#1610,.T.);
#1137=FACE_OUTER_BOUND('',#1611,.T.);
#1138=FACE_OUTER_BOUND('',#1612,.T.);
#1139=FACE_OUTER_BOUND('',#1613,.T.);
#1140=FACE_OUTER_BOUND('',#1614,.T.);
#1141=FACE_OUTER_BOUND('',#1615,.T.);
#1142=FACE_OUTER_BOUND('',#1616,.T.);
#1143=FACE_OUTER_BOUND('',#1617,.T.);
#1144=FACE_OUTER_BOUND('',#1618,.T.);
#1145=FACE_OUTER_BOUND('',#1619,.T.);
#1146=FACE_OUTER_BOUND('',#1620,.T.);
#1147=FACE_OUTER_BOUND('',#1621,.T.);
#1148=FACE_OUTER_BOUND('',#1622,.T.);
#1149=FACE_OUTER_BOUND('',#1623,.T.);
#1150=FACE_OUTER_BOUND('',#1624,.T.);
#1151=FACE_OUTER_BOUND('',#1625,.T.);
#1152=FACE_OUTER_BOUND('',#1626,.T.);
#1153=FACE_OUTER_BOUND('',#1627,.T.);
#1154=FACE_OUTER_BOUND('',#1628,.T.);
#1155=FACE_OUTER_BOUND('',#1629,.T.);
#1156=FACE_OUTER_BOUND('',#1630,.T.);
#1157=FACE_OUTER_BOUND('',#1631,.T.);
#1158=FACE_OUTER_BOUND('',#1632,.T.);
#1159=FACE_OUTER_BOUND('',#1633,.T.);
#1160=FACE_OUTER_BOUND('',#1634,.T.);
#1161=FACE_OUTER_BOUND('',#1635,.T.);
#1162=FACE_OUTER_BOUND('',#1636,.T.);
#1163=FACE_OUTER_BOUND('',#1637,.T.);
#1164=FACE_OUTER_BOUND('',#1638,.T.);
#1165=FACE_OUTER_BOUND('',#1639,.T.);
#1166=FACE_OUTER_BOUND('',#1640,.T.);
#1167=FACE_OUTER_BOUND('',#1641,.T.);
#1168=FACE_OUTER_BOUND('',#1642,.T.);
#1169=FACE_OUTER_BOUND('',#1643,.T.);
#1170=FACE_OUTER_BOUND('',#1644,.T.);
#1171=FACE_OUTER_BOUND('',#1645,.T.);
#1172=FACE_OUTER_BOUND('',#1646,.T.);
#1173=FACE_OUTER_BOUND('',#1647,.T.);
#1174=FACE_OUTER_BOUND('',#1648,.T.);
#1175=FACE_OUTER_BOUND('',#1649,.T.);
#1176=FACE_OUTER_BOUND('',#1650,.T.);
#1177=FACE_OUTER_BOUND('',#1651,.T.);
#1178=FACE_OUTER_BOUND('',#1652,.T.);
#1179=FACE_OUTER_BOUND('',#1653,.T.);
#1180=FACE_OUTER_BOUND('',#1654,.T.);
#1181=FACE_OUTER_BOUND('',#1655,.T.);
#1182=FACE_OUTER_BOUND('',#1656,.T.);
#1183=FACE_OUTER_BOUND('',#1657,.T.);
#1184=FACE_OUTER_BOUND('',#1658,.T.);
#1185=FACE_OUTER_BOUND('',#1659,.T.);
#1186=FACE_OUTER_BOUND('',#1660,.T.);
#1187=FACE_OUTER_BOUND('',#1661,.T.);
#1188=FACE_OUTER_BOUND('',#1662,.T.);
#1189=FACE_OUTER_BOUND('',#1663,.T.);
#1190=FACE_OUTER_BOUND('',#1664,.T.);
#1191=FACE_OUTER_BOUND('',#1665,.T.);
#1192=FACE_OUTER_BOUND('',#1666,.T.);
#1193=FACE_OUTER_BOUND('',#1667,.T.);
#1194=FACE_OUTER_BOUND('',#1668,.T.);
#1195=FACE_OUTER_BOUND('',#1669,.T.);
#1196=FACE_OUTER_BOUND('',#1670,.T.);
#1197=FACE_OUTER_BOUND('',#1671,.T.);
#1198=FACE_OUTER_BOUND('',#1672,.T.);
#1199=FACE_OUTER_BOUND('',#1673,.T.);
#1200=FACE_OUTER_BOUND('',#1675,.T.);
#1201=FACE_OUTER_BOUND('',#1676,.T.);
#1202=FACE_OUTER_BOUND('',#1678,.T.);
#1203=FACE_OUTER_BOUND('',#1679,.T.);
#1204=FACE_OUTER_BOUND('',#1680,.T.);
#1205=FACE_OUTER_BOUND('',#1681,.T.);
#1206=FACE_OUTER_BOUND('',#1682,.T.);
#1207=FACE_OUTER_BOUND('',#1683,.T.);
#1208=FACE_OUTER_BOUND('',#1684,.T.);
#1209=FACE_OUTER_BOUND('',#1685,.T.);
#1210=FACE_OUTER_BOUND('',#1686,.T.);
#1211=FACE_OUTER_BOUND('',#1687,.T.);
#1212=FACE_OUTER_BOUND('',#1688,.T.);
#1213=FACE_OUTER_BOUND('',#1689,.T.);
#1214=FACE_OUTER_BOUND('',#1690,.T.);
#1215=FACE_OUTER_BOUND('',#1691,.T.);
#1216=FACE_OUTER_BOUND('',#1692,.T.);
#1217=FACE_OUTER_BOUND('',#1694,.T.);
#1218=FACE_OUTER_BOUND('',#1695,.T.);
#1219=FACE_OUTER_BOUND('',#1696,.T.);
#1220=FACE_OUTER_BOUND('',#1697,.T.);
#1221=FACE_OUTER_BOUND('',#1698,.T.);
#1222=FACE_OUTER_BOUND('',#1699,.T.);
#1223=FACE_OUTER_BOUND('',#1700,.T.);
#1224=FACE_OUTER_BOUND('',#1701,.T.);
#1225=FACE_OUTER_BOUND('',#1703,.T.);
#1226=FACE_OUTER_BOUND('',#1704,.T.);
#1227=FACE_OUTER_BOUND('',#1705,.T.);
#1228=FACE_OUTER_BOUND('',#1707,.T.);
#1229=EDGE_LOOP('',(#4541,#4542,#4543,#4544));
#1230=EDGE_LOOP('',(#4545,#4546,#4547,#4548));
#1231=EDGE_LOOP('',(#4549,#4550,#4551,#4552));
#1232=EDGE_LOOP('',(#4553,#4554,#4555));
#1233=EDGE_LOOP('',(#4556,#4557,#4558,#4559));
#1234=EDGE_LOOP('',(#4560,#4561,#4562));
#1235=EDGE_LOOP('',(#4563,#4564,#4565,#4566,#4567,#4568,#4569,#4570));
#1236=EDGE_LOOP('',(#4571,#4572,#4573,#4574));
#1237=EDGE_LOOP('',(#4575,#4576,#4577,#4578));
#1238=EDGE_LOOP('',(#4579,#4580,#4581,#4582));
#1239=EDGE_LOOP('',(#4583,#4584,#4585,#4586,#4587,#4588));
#1240=EDGE_LOOP('',(#4589,#4590,#4591,#4592,#4593,#4594));
#1241=EDGE_LOOP('',(#4595,#4596,#4597,#4598,#4599,#4600,#4601,#4602));
#1242=EDGE_LOOP('',(#4603,#4604,#4605,#4606));
#1243=EDGE_LOOP('',(#4607,#4608));
#1244=EDGE_LOOP('',(#4609,#4610,#4611,#4612,#4613,#4614));
#1245=EDGE_LOOP('',(#4615,#4616,#4617,#4618,#4619,#4620,#4621,#4622,#4623,
#4624,#4625,#4626,#4627,#4628,#4629,#4630));
#1246=EDGE_LOOP('',(#4631));
#1247=EDGE_LOOP('',(#4632));
#1248=EDGE_LOOP('',(#4633));
#1249=EDGE_LOOP('',(#4634));
#1250=EDGE_LOOP('',(#4635,#4636,#4637,#4638));
#1251=EDGE_LOOP('',(#4639,#4640,#4641,#4642));
#1252=EDGE_LOOP('',(#4643,#4644,#4645,#4646));
#1253=EDGE_LOOP('',(#4647,#4648,#4649,#4650,#4651,#4652,#4653,#4654,#4655,
#4656,#4657,#4658,#4659,#4660,#4661,#4662));
#1254=EDGE_LOOP('',(#4663));
#1255=EDGE_LOOP('',(#4664));
#1256=EDGE_LOOP('',(#4665));
#1257=EDGE_LOOP('',(#4666));
#1258=EDGE_LOOP('',(#4667,#4668,#4669,#4670));
#1259=EDGE_LOOP('',(#4671,#4672,#4673,#4674,#4675));
#1260=EDGE_LOOP('',(#4676,#4677,#4678,#4679,#4680));
#1261=EDGE_LOOP('',(#4681,#4682,#4683,#4684));
#1262=EDGE_LOOP('',(#4685,#4686,#4687,#4688));
#1263=EDGE_LOOP('',(#4689,#4690,#4691,#4692));
#1264=EDGE_LOOP('',(#4693,#4694,#4695,#4696));
#1265=EDGE_LOOP('',(#4697,#4698,#4699,#4700));
#1266=EDGE_LOOP('',(#4701,#4702,#4703,#4704));
#1267=EDGE_LOOP('',(#4705,#4706,#4707,#4708));
#1268=EDGE_LOOP('',(#4709,#4710,#4711,#4712));
#1269=EDGE_LOOP('',(#4713,#4714,#4715,#4716));
#1270=EDGE_LOOP('',(#4717,#4718,#4719,#4720));
#1271=EDGE_LOOP('',(#4721,#4722,#4723,#4724));
#1272=EDGE_LOOP('',(#4725,#4726,#4727,#4728));
#1273=EDGE_LOOP('',(#4729,#4730,#4731,#4732));
#1274=EDGE_LOOP('',(#4733,#4734,#4735));
#1275=EDGE_LOOP('',(#4736,#4737,#4738,#4739));
#1276=EDGE_LOOP('',(#4740,#4741,#4742));
#1277=EDGE_LOOP('',(#4743,#4744,#4745,#4746,#4747,#4748));
#1278=EDGE_LOOP('',(#4749,#4750));
#1279=EDGE_LOOP('',(#4751,#4752,#4753,#4754));
#1280=EDGE_LOOP('',(#4755,#4756,#4757,#4758));
#1281=EDGE_LOOP('',(#4759,#4760,#4761,#4762));
#1282=EDGE_LOOP('',(#4763,#4764,#4765,#4766,#4767,#4768,#4769,#4770));
#1283=EDGE_LOOP('',(#4771,#4772,#4773,#4774));
#1284=EDGE_LOOP('',(#4775,#4776,#4777,#4778,#4779,#4780));
#1285=EDGE_LOOP('',(#4781,#4782,#4783,#4784,#4785,#4786,#4787,#4788,#4789,
#4790,#4791,#4792,#4793,#4794,#4795,#4796));
#1286=EDGE_LOOP('',(#4797));
#1287=EDGE_LOOP('',(#4798));
#1288=EDGE_LOOP('',(#4799));
#1289=EDGE_LOOP('',(#4800));
#1290=EDGE_LOOP('',(#4801,#4802,#4803,#4804,#4805,#4806,#4807,#4808));
#1291=EDGE_LOOP('',(#4809,#4810,#4811,#4812,#4813,#4814));
#1292=EDGE_LOOP('',(#4815,#4816,#4817,#4818));
#1293=EDGE_LOOP('',(#4819,#4820,#4821,#4822));
#1294=EDGE_LOOP('',(#4823,#4824,#4825,#4826));
#1295=EDGE_LOOP('',(#4827,#4828,#4829,#4830,#4831,#4832,#4833,#4834,#4835,
#4836,#4837,#4838,#4839,#4840,#4841,#4842));
#1296=EDGE_LOOP('',(#4843));
#1297=EDGE_LOOP('',(#4844));
#1298=EDGE_LOOP('',(#4845));
#1299=EDGE_LOOP('',(#4846));
#1300=EDGE_LOOP('',(#4847,#4848,#4849,#4850));
#1301=EDGE_LOOP('',(#4851,#4852,#4853,#4854,#4855));
#1302=EDGE_LOOP('',(#4856,#4857,#4858,#4859,#4860));
#1303=EDGE_LOOP('',(#4861,#4862,#4863,#4864));
#1304=EDGE_LOOP('',(#4865,#4866,#4867,#4868));
#1305=EDGE_LOOP('',(#4869,#4870,#4871,#4872));
#1306=EDGE_LOOP('',(#4873,#4874,#4875,#4876));
#1307=EDGE_LOOP('',(#4877,#4878,#4879,#4880));
#1308=EDGE_LOOP('',(#4881,#4882,#4883,#4884));
#1309=EDGE_LOOP('',(#4885,#4886,#4887,#4888));
#1310=EDGE_LOOP('',(#4889,#4890,#4891,#4892));
#1311=EDGE_LOOP('',(#4893,#4894,#4895,#4896));
#1312=EDGE_LOOP('',(#4897,#4898,#4899,#4900));
#1313=EDGE_LOOP('',(#4901,#4902,#4903,#4904));
#1314=EDGE_LOOP('',(#4905));
#1315=EDGE_LOOP('',(#4906));
#1316=EDGE_LOOP('',(#4907));
#1317=EDGE_LOOP('',(#4908));
#1318=EDGE_LOOP('',(#4909,#4910,#4911,#4912));
#1319=EDGE_LOOP('',(#4913));
#1320=EDGE_LOOP('',(#4914));
#1321=EDGE_LOOP('',(#4915,#4916,#4917,#4918));
#1322=EDGE_LOOP('',(#4919));
#1323=EDGE_LOOP('',(#4920,#4921,#4922,#4923));
#1324=EDGE_LOOP('',(#4924));
#1325=EDGE_LOOP('',(#4925,#4926,#4927,#4928));
#1326=EDGE_LOOP('',(#4929,#4930,#4931,#4932));
#1327=EDGE_LOOP('',(#4933,#4934,#4935,#4936));
#1328=EDGE_LOOP('',(#4937,#4938,#4939,#4940));
#1329=EDGE_LOOP('',(#4941,#4942,#4943,#4944));
#1330=EDGE_LOOP('',(#4945,#4946,#4947,#4948));
#1331=EDGE_LOOP('',(#4949,#4950,#4951,#4952));
#1332=EDGE_LOOP('',(#4953,#4954,#4955,#4956));
#1333=EDGE_LOOP('',(#4957,#4958,#4959,#4960));
#1334=EDGE_LOOP('',(#4961,#4962,#4963,#4964));
#1335=EDGE_LOOP('',(#4965,#4966,#4967,#4968));
#1336=EDGE_LOOP('',(#4969));
#1337=EDGE_LOOP('',(#4970));
#1338=EDGE_LOOP('',(#4971,#4972,#4973,#4974));
#1339=EDGE_LOOP('',(#4975));
#1340=EDGE_LOOP('',(#4976));
#1341=EDGE_LOOP('',(#4977,#4978,#4979,#4980));
#1342=EDGE_LOOP('',(#4981,#4982,#4983,#4984));
#1343=EDGE_LOOP('',(#4985,#4986,#4987,#4988));
#1344=EDGE_LOOP('',(#4989,#4990,#4991,#4992));
#1345=EDGE_LOOP('',(#4993,#4994,#4995,#4996));
#1346=EDGE_LOOP('',(#4997,#4998,#4999,#5000));
#1347=EDGE_LOOP('',(#5001,#5002,#5003,#5004));
#1348=EDGE_LOOP('',(#5005,#5006,#5007,#5008));
#1349=EDGE_LOOP('',(#5009,#5010,#5011,#5012));
#1350=EDGE_LOOP('',(#5013));
#1351=EDGE_LOOP('',(#5014));
#1352=EDGE_LOOP('',(#5015));
#1353=EDGE_LOOP('',(#5016));
#1354=EDGE_LOOP('',(#5017,#5018,#5019,#5020));
#1355=EDGE_LOOP('',(#5021,#5022,#5023,#5024));
#1356=EDGE_LOOP('',(#5025,#5026,#5027,#5028));
#1357=EDGE_LOOP('',(#5029,#5030,#5031,#5032));
#1358=EDGE_LOOP('',(#5033,#5034,#5035,#5036));
#1359=EDGE_LOOP('',(#5037,#5038,#5039,#5040,#5041,#5042));
#1360=EDGE_LOOP('',(#5043,#5044,#5045,#5046,#5047,#5048,#5049,#5050,#5051,
#5052));
#1361=EDGE_LOOP('',(#5053,#5054,#5055,#5056,#5057,#5058,#5059,#5060,#5061,
#5062));
#1362=EDGE_LOOP('',(#5063,#5064,#5065,#5066,#5067,#5068,#5069,#5070,#5071,
#5072));
#1363=EDGE_LOOP('',(#5073,#5074,#5075,#5076,#5077,#5078,#5079,#5080));
#1364=EDGE_LOOP('',(#5081,#5082,#5083,#5084,#5085,#5086,#5087,#5088,#5089,
#5090,#5091,#5092,#5093,#5094,#5095,#5096,#5097,#5098,#5099,#5100,#5101,
#5102,#5103,#5104,#5105,#5106,#5107,#5108,#5109,#5110,#5111,#5112,#5113,
#5114,#5115,#5116,#5117,#5118,#5119,#5120,#5121,#5122));
#1365=EDGE_LOOP('',(#5123,#5124,#5125,#5126,#5127,#5128));
#1366=EDGE_LOOP('',(#5129,#5130,#5131,#5132));
#1367=EDGE_LOOP('',(#5133,#5134,#5135,#5136));
#1368=EDGE_LOOP('',(#5137,#5138,#5139,#5140,#5141,#5142));
#1369=EDGE_LOOP('',(#5143,#5144,#5145,#5146));
#1370=EDGE_LOOP('',(#5147,#5148,#5149,#5150));
#1371=EDGE_LOOP('',(#5151,#5152,#5153,#5154));
#1372=EDGE_LOOP('',(#5155,#5156,#5157,#5158));
#1373=EDGE_LOOP('',(#5159,#5160,#5161,#5162));
#1374=EDGE_LOOP('',(#5163));
#1375=EDGE_LOOP('',(#5164));
#1376=EDGE_LOOP('',(#5165));
#1377=EDGE_LOOP('',(#5166,#5167,#5168,#5169));
#1378=EDGE_LOOP('',(#5170,#5171,#5172,#5173));
#1379=EDGE_LOOP('',(#5174,#5175,#5176,#5177));
#1380=EDGE_LOOP('',(#5178,#5179,#5180,#5181));
#1381=EDGE_LOOP('',(#5182,#5183,#5184,#5185,#5186,#5187,#5188,#5189,#5190,
#5191));
#1382=EDGE_LOOP('',(#5192,#5193,#5194,#5195));
#1383=EDGE_LOOP('',(#5196,#5197,#5198,#5199));
#1384=EDGE_LOOP('',(#5200,#5201,#5202,#5203));
#1385=EDGE_LOOP('',(#5204,#5205,#5206,#5207));
#1386=EDGE_LOOP('',(#5208,#5209,#5210,#5211));
#1387=EDGE_LOOP('',(#5212,#5213,#5214,#5215,#5216,#5217,#5218,#5219,#5220,
#5221));
#1388=EDGE_LOOP('',(#5222,#5223,#5224,#5225));
#1389=EDGE_LOOP('',(#5226,#5227,#5228,#5229));
#1390=EDGE_LOOP('',(#5230,#5231,#5232,#5233));
#1391=EDGE_LOOP('',(#5234));
#1392=EDGE_LOOP('',(#5235));
#1393=EDGE_LOOP('',(#5236));
#1394=EDGE_LOOP('',(#5237,#5238,#5239,#5240));
#1395=EDGE_LOOP('',(#5241,#5242,#5243,#5244));
#1396=EDGE_LOOP('',(#5245,#5246,#5247,#5248,#5249,#5250,#5251,#5252,#5253,
#5254));
#1397=EDGE_LOOP('',(#5255,#5256,#5257,#5258));
#1398=EDGE_LOOP('',(#5259,#5260,#5261,#5262));
#1399=EDGE_LOOP('',(#5263,#5264,#5265,#5266));
#1400=EDGE_LOOP('',(#5267,#5268,#5269,#5270));
#1401=EDGE_LOOP('',(#5271,#5272,#5273,#5274));
#1402=EDGE_LOOP('',(#5275,#5276,#5277));
#1403=EDGE_LOOP('',(#5278,#5279,#5280));
#1404=EDGE_LOOP('',(#5281,#5282,#5283));
#1405=EDGE_LOOP('',(#5284,#5285,#5286,#5287));
#1406=EDGE_LOOP('',(#5288,#5289,#5290,#5291));
#1407=EDGE_LOOP('',(#5292,#5293,#5294));
#1408=EDGE_LOOP('',(#5295,#5296,#5297,#5298));
#1409=EDGE_LOOP('',(#5299,#5300,#5301,#5302));
#1410=EDGE_LOOP('',(#5303,#5304,#5305,#5306));
#1411=EDGE_LOOP('',(#5307,#5308,#5309,#5310));
#1412=EDGE_LOOP('',(#5311,#5312,#5313,#5314));
#1413=EDGE_LOOP('',(#5315,#5316,#5317,#5318));
#1414=EDGE_LOOP('',(#5319,#5320,#5321));
#1415=EDGE_LOOP('',(#5322,#5323,#5324));
#1416=EDGE_LOOP('',(#5325,#5326,#5327));
#1417=EDGE_LOOP('',(#5328,#5329,#5330,#5331));
#1418=EDGE_LOOP('',(#5332,#5333,#5334,#5335));
#1419=EDGE_LOOP('',(#5336,#5337,#5338));
#1420=EDGE_LOOP('',(#5339,#5340,#5341,#5342));
#1421=EDGE_LOOP('',(#5343,#5344,#5345,#5346));
#1422=EDGE_LOOP('',(#5347,#5348,#5349,#5350));
#1423=EDGE_LOOP('',(#5351,#5352,#5353,#5354));
#1424=EDGE_LOOP('',(#5355,#5356,#5357,#5358));
#1425=EDGE_LOOP('',(#5359,#5360,#5361,#5362));
#1426=EDGE_LOOP('',(#5363,#5364,#5365,#5366));
#1427=EDGE_LOOP('',(#5367,#5368,#5369,#5370,#5371,#5372,#5373,#5374));
#1428=EDGE_LOOP('',(#5375,#5376,#5377,#5378));
#1429=EDGE_LOOP('',(#5379));
#1430=EDGE_LOOP('',(#5380));
#1431=EDGE_LOOP('',(#5381));
#1432=EDGE_LOOP('',(#5382));
#1433=EDGE_LOOP('',(#5383));
#1434=EDGE_LOOP('',(#5384));
#1435=EDGE_LOOP('',(#5385,#5386,#5387,#5388));
#1436=EDGE_LOOP('',(#5389,#5390,#5391,#5392));
#1437=EDGE_LOOP('',(#5393,#5394,#5395,#5396));
#1438=EDGE_LOOP('',(#5397,#5398,#5399,#5400));
#1439=EDGE_LOOP('',(#5401,#5402,#5403,#5404));
#1440=EDGE_LOOP('',(#5405,#5406,#5407,#5408));
#1441=EDGE_LOOP('',(#5409,#5410,#5411,#5412));
#1442=EDGE_LOOP('',(#5413,#5414,#5415,#5416));
#1443=EDGE_LOOP('',(#5417,#5418,#5419,#5420));
#1444=EDGE_LOOP('',(#5421,#5422,#5423,#5424));
#1445=EDGE_LOOP('',(#5425,#5426,#5427,#5428));
#1446=EDGE_LOOP('',(#5429,#5430,#5431,#5432));
#1447=EDGE_LOOP('',(#5433,#5434,#5435,#5436,#5437,#5438));
#1448=EDGE_LOOP('',(#5439));
#1449=EDGE_LOOP('',(#5440,#5441,#5442,#5443));
#1450=EDGE_LOOP('',(#5444,#5445,#5446,#5447));
#1451=EDGE_LOOP('',(#5448,#5449,#5450,#5451));
#1452=EDGE_LOOP('',(#5452,#5453,#5454,#5455));
#1453=EDGE_LOOP('',(#5456,#5457,#5458,#5459));
#1454=EDGE_LOOP('',(#5460,#5461,#5462,#5463));
#1455=EDGE_LOOP('',(#5464,#5465,#5466,#5467,#5468,#5469));
#1456=EDGE_LOOP('',(#5470));
#1457=EDGE_LOOP('',(#5471,#5472,#5473,#5474));
#1458=EDGE_LOOP('',(#5475,#5476,#5477,#5478));
#1459=EDGE_LOOP('',(#5479,#5480,#5481,#5482));
#1460=EDGE_LOOP('',(#5483,#5484,#5485,#5486));
#1461=EDGE_LOOP('',(#5487,#5488,#5489,#5490));
#1462=EDGE_LOOP('',(#5491,#5492,#5493,#5494));
#1463=EDGE_LOOP('',(#5495,#5496,#5497,#5498));
#1464=EDGE_LOOP('',(#5499,#5500,#5501,#5502));
#1465=EDGE_LOOP('',(#5503,#5504,#5505,#5506));
#1466=EDGE_LOOP('',(#5507));
#1467=EDGE_LOOP('',(#5508));
#1468=EDGE_LOOP('',(#5509));
#1469=EDGE_LOOP('',(#5510));
#1470=EDGE_LOOP('',(#5511,#5512,#5513,#5514));
#1471=EDGE_LOOP('',(#5515,#5516,#5517,#5518));
#1472=EDGE_LOOP('',(#5519,#5520,#5521,#5522));
#1473=EDGE_LOOP('',(#5523,#5524,#5525,#5526));
#1474=EDGE_LOOP('',(#5527,#5528,#5529,#5530));
#1475=EDGE_LOOP('',(#5531,#5532,#5533,#5534,#5535,#5536));
#1476=EDGE_LOOP('',(#5537,#5538,#5539,#5540,#5541,#5542,#5543,#5544,#5545,
#5546));
#1477=EDGE_LOOP('',(#5547,#5548,#5549,#5550,#5551,#5552,#5553,#5554,#5555,
#5556));
#1478=EDGE_LOOP('',(#5557,#5558,#5559,#5560,#5561,#5562,#5563,#5564,#5565,
#5566));
#1479=EDGE_LOOP('',(#5567,#5568,#5569,#5570,#5571,#5572,#5573,#5574));
#1480=EDGE_LOOP('',(#5575,#5576,#5577,#5578,#5579,#5580,#5581,#5582,#5583,
#5584,#5585,#5586,#5587,#5588,#5589,#5590,#5591,#5592,#5593,#5594,#5595,
#5596,#5597,#5598,#5599,#5600,#5601,#5602,#5603,#5604,#5605,#5606,#5607,
#5608,#5609,#5610,#5611,#5612,#5613,#5614,#5615,#5616));
#1481=EDGE_LOOP('',(#5617,#5618,#5619,#5620,#5621,#5622));
#1482=EDGE_LOOP('',(#5623,#5624,#5625,#5626));
#1483=EDGE_LOOP('',(#5627,#5628,#5629,#5630));
#1484=EDGE_LOOP('',(#5631,#5632,#5633,#5634,#5635,#5636));
#1485=EDGE_LOOP('',(#5637,#5638,#5639,#5640));
#1486=EDGE_LOOP('',(#5641,#5642,#5643,#5644));
#1487=EDGE_LOOP('',(#5645,#5646,#5647,#5648));
#1488=EDGE_LOOP('',(#5649,#5650,#5651,#5652));
#1489=EDGE_LOOP('',(#5653,#5654,#5655,#5656));
#1490=EDGE_LOOP('',(#5657));
#1491=EDGE_LOOP('',(#5658));
#1492=EDGE_LOOP('',(#5659));
#1493=EDGE_LOOP('',(#5660,#5661,#5662,#5663));
#1494=EDGE_LOOP('',(#5664,#5665,#5666,#5667));
#1495=EDGE_LOOP('',(#5668,#5669,#5670,#5671));
#1496=EDGE_LOOP('',(#5672,#5673,#5674,#5675));
#1497=EDGE_LOOP('',(#5676,#5677,#5678,#5679,#5680,#5681,#5682,#5683,#5684,
#5685));
#1498=EDGE_LOOP('',(#5686,#5687,#5688,#5689));
#1499=EDGE_LOOP('',(#5690,#5691,#5692,#5693));
#1500=EDGE_LOOP('',(#5694,#5695,#5696,#5697));
#1501=EDGE_LOOP('',(#5698,#5699,#5700,#5701));
#1502=EDGE_LOOP('',(#5702,#5703,#5704,#5705));
#1503=EDGE_LOOP('',(#5706,#5707,#5708,#5709,#5710,#5711,#5712,#5713,#5714,
#5715));
#1504=EDGE_LOOP('',(#5716,#5717,#5718,#5719));
#1505=EDGE_LOOP('',(#5720,#5721,#5722,#5723));
#1506=EDGE_LOOP('',(#5724,#5725,#5726,#5727));
#1507=EDGE_LOOP('',(#5728));
#1508=EDGE_LOOP('',(#5729));
#1509=EDGE_LOOP('',(#5730));
#1510=EDGE_LOOP('',(#5731,#5732,#5733,#5734));
#1511=EDGE_LOOP('',(#5735,#5736,#5737,#5738));
#1512=EDGE_LOOP('',(#5739,#5740,#5741,#5742,#5743,#5744,#5745,#5746,#5747,
#5748));
#1513=EDGE_LOOP('',(#5749,#5750,#5751,#5752));
#1514=EDGE_LOOP('',(#5753,#5754,#5755,#5756));
#1515=EDGE_LOOP('',(#5757,#5758,#5759,#5760));
#1516=EDGE_LOOP('',(#5761,#5762,#5763,#5764));
#1517=EDGE_LOOP('',(#5765,#5766,#5767,#5768));
#1518=EDGE_LOOP('',(#5769,#5770,#5771));
#1519=EDGE_LOOP('',(#5772,#5773,#5774));
#1520=EDGE_LOOP('',(#5775,#5776,#5777));
#1521=EDGE_LOOP('',(#5778,#5779,#5780,#5781));
#1522=EDGE_LOOP('',(#5782,#5783,#5784,#5785));
#1523=EDGE_LOOP('',(#5786,#5787,#5788));
#1524=EDGE_LOOP('',(#5789,#5790,#5791,#5792));
#1525=EDGE_LOOP('',(#5793,#5794,#5795,#5796));
#1526=EDGE_LOOP('',(#5797,#5798,#5799,#5800));
#1527=EDGE_LOOP('',(#5801,#5802,#5803,#5804));
#1528=EDGE_LOOP('',(#5805,#5806,#5807,#5808));
#1529=EDGE_LOOP('',(#5809,#5810,#5811,#5812));
#1530=EDGE_LOOP('',(#5813,#5814,#5815));
#1531=EDGE_LOOP('',(#5816,#5817,#5818));
#1532=EDGE_LOOP('',(#5819,#5820,#5821));
#1533=EDGE_LOOP('',(#5822,#5823,#5824,#5825));
#1534=EDGE_LOOP('',(#5826,#5827,#5828,#5829));
#1535=EDGE_LOOP('',(#5830,#5831,#5832));
#1536=EDGE_LOOP('',(#5833,#5834,#5835,#5836));
#1537=EDGE_LOOP('',(#5837,#5838,#5839,#5840));
#1538=EDGE_LOOP('',(#5841,#5842,#5843,#5844));
#1539=EDGE_LOOP('',(#5845,#5846,#5847,#5848));
#1540=EDGE_LOOP('',(#5849,#5850,#5851,#5852));
#1541=EDGE_LOOP('',(#5853,#5854,#5855,#5856));
#1542=EDGE_LOOP('',(#5857,#5858,#5859,#5860));
#1543=EDGE_LOOP('',(#5861,#5862,#5863,#5864,#5865,#5866,#5867,#5868));
#1544=EDGE_LOOP('',(#5869,#5870,#5871,#5872));
#1545=EDGE_LOOP('',(#5873,#5874,#5875,#5876,#5877,#5878));
#1546=EDGE_LOOP('',(#5879,#5880,#5881,#5882,#5883,#5884));
#1547=EDGE_LOOP('',(#5885));
#1548=EDGE_LOOP('',(#5886));
#1549=EDGE_LOOP('',(#5887));
#1550=EDGE_LOOP('',(#5888));
#1551=EDGE_LOOP('',(#5889,#5890,#5891,#5892));
#1552=EDGE_LOOP('',(#5893,#5894,#5895,#5896));
#1553=EDGE_LOOP('',(#5897,#5898,#5899,#5900));
#1554=EDGE_LOOP('',(#5901,#5902,#5903,#5904));
#1555=EDGE_LOOP('',(#5905));
#1556=EDGE_LOOP('',(#5906));
#1557=EDGE_LOOP('',(#5907,#5908,#5909,#5910));
#1558=EDGE_LOOP('',(#5911));
#1559=EDGE_LOOP('',(#5912));
#1560=EDGE_LOOP('',(#5913));
#1561=EDGE_LOOP('',(#5914,#5915,#5916,#5917));
#1562=EDGE_LOOP('',(#5918));
#1563=EDGE_LOOP('',(#5919));
#1564=EDGE_LOOP('',(#5920));
#1565=EDGE_LOOP('',(#5921,#5922,#5923,#5924));
#1566=EDGE_LOOP('',(#5925));
#1567=EDGE_LOOP('',(#5926));
#1568=EDGE_LOOP('',(#5927));
#1569=EDGE_LOOP('',(#5928,#5929,#5930,#5931));
#1570=EDGE_LOOP('',(#5932));
#1571=EDGE_LOOP('',(#5933,#5934,#5935,#5936));
#1572=EDGE_LOOP('',(#5937,#5938,#5939,#5940));
#1573=EDGE_LOOP('',(#5941,#5942,#5943,#5944));
#1574=EDGE_LOOP('',(#5945,#5946,#5947,#5948));
#1575=EDGE_LOOP('',(#5949,#5950,#5951,#5952));
#1576=EDGE_LOOP('',(#5953,#5954,#5955,#5956));
#1577=EDGE_LOOP('',(#5957,#5958,#5959,#5960));
#1578=EDGE_LOOP('',(#5961,#5962,#5963,#5964));
#1579=EDGE_LOOP('',(#5965,#5966,#5967,#5968));
#1580=EDGE_LOOP('',(#5969,#5970,#5971,#5972));
#1581=EDGE_LOOP('',(#5973,#5974,#5975,#5976));
#1582=EDGE_LOOP('',(#5977,#5978,#5979,#5980));
#1583=EDGE_LOOP('',(#5981,#5982,#5983,#5984));
#1584=EDGE_LOOP('',(#5985,#5986,#5987,#5988));
#1585=EDGE_LOOP('',(#5989,#5990,#5991,#5992));
#1586=EDGE_LOOP('',(#5993,#5994,#5995,#5996));
#1587=EDGE_LOOP('',(#5997,#5998,#5999,#6000,#6001,#6002,#6003,#6004));
#1588=EDGE_LOOP('',(#6005));
#1589=EDGE_LOOP('',(#6006));
#1590=EDGE_LOOP('',(#6007,#6008,#6009,#6010));
#1591=EDGE_LOOP('',(#6011,#6012,#6013,#6014));
#1592=EDGE_LOOP('',(#6015,#6016,#6017,#6018));
#1593=EDGE_LOOP('',(#6019,#6020,#6021,#6022,#6023,#6024,#6025,#6026));
#1594=EDGE_LOOP('',(#6027));
#1595=EDGE_LOOP('',(#6028));
#1596=EDGE_LOOP('',(#6029));
#1597=EDGE_LOOP('',(#6030));
#1598=EDGE_LOOP('',(#6031));
#1599=EDGE_LOOP('',(#6032));
#1600=EDGE_LOOP('',(#6033,#6034,#6035,#6036));
#1601=EDGE_LOOP('',(#6037,#6038,#6039,#6040));
#1602=EDGE_LOOP('',(#6041,#6042,#6043,#6044));
#1603=EDGE_LOOP('',(#6045,#6046,#6047,#6048));
#1604=EDGE_LOOP('',(#6049,#6050,#6051,#6052));
#1605=EDGE_LOOP('',(#6053,#6054,#6055,#6056));
#1606=EDGE_LOOP('',(#6057,#6058,#6059,#6060));
#1607=EDGE_LOOP('',(#6061,#6062,#6063,#6064));
#1608=EDGE_LOOP('',(#6065,#6066,#6067,#6068));
#1609=EDGE_LOOP('',(#6069,#6070,#6071,#6072));
#1610=EDGE_LOOP('',(#6073,#6074,#6075,#6076));
#1611=EDGE_LOOP('',(#6077,#6078,#6079,#6080));
#1612=EDGE_LOOP('',(#6081,#6082,#6083,#6084));
#1613=EDGE_LOOP('',(#6085,#6086,#6087,#6088));
#1614=EDGE_LOOP('',(#6089,#6090,#6091,#6092));
#1615=EDGE_LOOP('',(#6093,#6094,#6095,#6096));
#1616=EDGE_LOOP('',(#6097,#6098,#6099,#6100));
#1617=EDGE_LOOP('',(#6101,#6102,#6103,#6104));
#1618=EDGE_LOOP('',(#6105,#6106,#6107,#6108));
#1619=EDGE_LOOP('',(#6109,#6110,#6111,#6112));
#1620=EDGE_LOOP('',(#6113,#6114,#6115,#6116));
#1621=EDGE_LOOP('',(#6117,#6118,#6119,#6120));
#1622=EDGE_LOOP('',(#6121,#6122,#6123,#6124));
#1623=EDGE_LOOP('',(#6125,#6126,#6127,#6128));
#1624=EDGE_LOOP('',(#6129,#6130,#6131,#6132));
#1625=EDGE_LOOP('',(#6133,#6134,#6135,#6136));
#1626=EDGE_LOOP('',(#6137,#6138,#6139,#6140));
#1627=EDGE_LOOP('',(#6141,#6142,#6143,#6144));
#1628=EDGE_LOOP('',(#6145,#6146,#6147,#6148));
#1629=EDGE_LOOP('',(#6149,#6150,#6151,#6152));
#1630=EDGE_LOOP('',(#6153,#6154,#6155,#6156));
#1631=EDGE_LOOP('',(#6157,#6158,#6159,#6160));
#1632=EDGE_LOOP('',(#6161,#6162,#6163,#6164));
#1633=EDGE_LOOP('',(#6165,#6166,#6167,#6168));
#1634=EDGE_LOOP('',(#6169,#6170,#6171,#6172));
#1635=EDGE_LOOP('',(#6173,#6174,#6175,#6176));
#1636=EDGE_LOOP('',(#6177,#6178,#6179,#6180));
#1637=EDGE_LOOP('',(#6181,#6182,#6183,#6184));
#1638=EDGE_LOOP('',(#6185,#6186,#6187,#6188));
#1639=EDGE_LOOP('',(#6189,#6190,#6191,#6192));
#1640=EDGE_LOOP('',(#6193,#6194,#6195,#6196));
#1641=EDGE_LOOP('',(#6197,#6198,#6199,#6200));
#1642=EDGE_LOOP('',(#6201,#6202,#6203,#6204));
#1643=EDGE_LOOP('',(#6205,#6206,#6207,#6208));
#1644=EDGE_LOOP('',(#6209,#6210,#6211,#6212));
#1645=EDGE_LOOP('',(#6213,#6214,#6215,#6216));
#1646=EDGE_LOOP('',(#6217,#6218,#6219,#6220));
#1647=EDGE_LOOP('',(#6221,#6222,#6223,#6224));
#1648=EDGE_LOOP('',(#6225,#6226,#6227,#6228));
#1649=EDGE_LOOP('',(#6229,#6230,#6231,#6232));
#1650=EDGE_LOOP('',(#6233,#6234,#6235,#6236));
#1651=EDGE_LOOP('',(#6237,#6238,#6239,#6240));
#1652=EDGE_LOOP('',(#6241,#6242,#6243,#6244));
#1653=EDGE_LOOP('',(#6245,#6246,#6247,#6248));
#1654=EDGE_LOOP('',(#6249,#6250,#6251,#6252));
#1655=EDGE_LOOP('',(#6253,#6254,#6255,#6256));
#1656=EDGE_LOOP('',(#6257,#6258,#6259,#6260));
#1657=EDGE_LOOP('',(#6261,#6262,#6263,#6264));
#1658=EDGE_LOOP('',(#6265,#6266,#6267,#6268));
#1659=EDGE_LOOP('',(#6269,#6270,#6271,#6272));
#1660=EDGE_LOOP('',(#6273,#6274,#6275,#6276));
#1661=EDGE_LOOP('',(#6277,#6278,#6279,#6280,#6281,#6282,#6283,#6284));
#1662=EDGE_LOOP('',(#6285,#6286,#6287,#6288,#6289,#6290,#6291,#6292,#6293,
#6294,#6295,#6296,#6297,#6298,#6299,#6300,#6301,#6302,#6303,#6304,#6305,
#6306,#6307,#6308,#6309,#6310,#6311,#6312,#6313,#6314,#6315,#6316,#6317,
#6318,#6319,#6320,#6321,#6322,#6323,#6324,#6325,#6326,#6327,#6328,#6329,
#6330,#6331,#6332,#6333,#6334,#6335,#6336,#6337,#6338,#6339,#6340,#6341,
#6342,#6343,#6344,#6345,#6346,#6347,#6348));
#1663=EDGE_LOOP('',(#6349,#6350,#6351,#6352));
#1664=EDGE_LOOP('',(#6353,#6354,#6355,#6356,#6357,#6358,#6359,#6360,#6361,
#6362,#6363,#6364,#6365,#6366,#6367,#6368,#6369,#6370,#6371,#6372,#6373,
#6374,#6375,#6376,#6377,#6378,#6379,#6380,#6381,#6382,#6383,#6384,#6385,
#6386,#6387,#6388,#6389,#6390,#6391,#6392,#6393,#6394,#6395,#6396,#6397,
#6398,#6399,#6400,#6401,#6402,#6403,#6404,#6405,#6406,#6407,#6408,#6409,
#6410,#6411,#6412,#6413,#6414,#6415,#6416,#6417));
#1665=EDGE_LOOP('',(#6418,#6419,#6420,#6421));
#1666=EDGE_LOOP('',(#6422,#6423,#6424,#6425));
#1667=EDGE_LOOP('',(#6426,#6427,#6428,#6429));
#1668=EDGE_LOOP('',(#6430,#6431,#6432,#6433));
#1669=EDGE_LOOP('',(#6434,#6435,#6436,#6437));
#1670=EDGE_LOOP('',(#6438,#6439,#6440,#6441));
#1671=EDGE_LOOP('',(#6442,#6443,#6444,#6445));
#1672=EDGE_LOOP('',(#6446,#6447,#6448,#6449,#6450,#6451));
#1673=EDGE_LOOP('',(#6452));
#1674=EDGE_LOOP('',(#6453,#6454,#6455,#6456));
#1675=EDGE_LOOP('',(#6457,#6458,#6459,#6460));
#1676=EDGE_LOOP('',(#6461));
#1677=EDGE_LOOP('',(#6462,#6463,#6464,#6465,#6466,#6467));
#1678=EDGE_LOOP('',(#6468));
#1679=EDGE_LOOP('',(#6469,#6470,#6471));
#1680=EDGE_LOOP('',(#6472,#6473,#6474,#6475,#6476));
#1681=EDGE_LOOP('',(#6477,#6478,#6479,#6480));
#1682=EDGE_LOOP('',(#6481,#6482,#6483,#6484));
#1683=EDGE_LOOP('',(#6485,#6486,#6487,#6488));
#1684=EDGE_LOOP('',(#6489,#6490,#6491,#6492));
#1685=EDGE_LOOP('',(#6493,#6494,#6495,#6496));
#1686=EDGE_LOOP('',(#6497,#6498,#6499,#6500));
#1687=EDGE_LOOP('',(#6501,#6502,#6503,#6504));
#1688=EDGE_LOOP('',(#6505,#6506,#6507,#6508));
#1689=EDGE_LOOP('',(#6509,#6510,#6511,#6512));
#1690=EDGE_LOOP('',(#6513,#6514,#6515,#6516,#6517,#6518,#6519,#6520,#6521,
#6522,#6523,#6524,#6525,#6526));
#1691=EDGE_LOOP('',(#6527,#6528,#6529,#6530,#6531,#6532,#6533,#6534,#6535,
#6536,#6537,#6538,#6539));
#1692=EDGE_LOOP('',(#6540,#6541,#6542,#6543,#6544,#6545));
#1693=EDGE_LOOP('',(#6546,#6547,#6548,#6549));
#1694=EDGE_LOOP('',(#6550,#6551,#6552,#6553));
#1695=EDGE_LOOP('',(#6554,#6555,#6556,#6557));
#1696=EDGE_LOOP('',(#6558,#6559,#6560,#6561));
#1697=EDGE_LOOP('',(#6562,#6563,#6564,#6565));
#1698=EDGE_LOOP('',(#6566,#6567,#6568,#6569));
#1699=EDGE_LOOP('',(#6570,#6571,#6572,#6573));
#1700=EDGE_LOOP('',(#6574,#6575,#6576,#6577));
#1701=EDGE_LOOP('',(#6578,#6579,#6580,#6581,#6582,#6583));
#1702=EDGE_LOOP('',(#6584,#6585,#6586,#6587,#6588));
#1703=EDGE_LOOP('',(#6589,#6590,#6591,#6592));
#1704=EDGE_LOOP('',(#6593,#6594,#6595,#6596));
#1705=EDGE_LOOP('',(#6597));
#1706=EDGE_LOOP('',(#6598));
#1707=EDGE_LOOP('',(#6599));
#1708=EDGE_LOOP('',(#6600));
#1709=LINE('',#9393,#2183);
#1710=LINE('',#9399,#2184);
#1711=LINE('',#9405,#2185);
#1712=LINE('',#9410,#2186);
#1713=LINE('',#9412,#2187);
#1714=LINE('',#9413,#2188);
#1715=LINE('',#9417,#2189);
#1716=LINE('',#9418,#2190);
#1717=LINE('',#9419,#2191);
#1718=LINE('',#9422,#2192);
#1719=LINE('',#9423,#2193);
#1720=LINE('',#9426,#2194);
#1721=LINE('',#9428,#2195);
#1722=LINE('',#9430,#2196);
#1723=LINE('',#9432,#2197);
#1724=LINE('',#9434,#2198);
#1725=LINE('',#9438,#2199);
#1726=LINE('',#9439,#2200);
#1727=LINE('',#9444,#2201);
#1728=LINE('',#9448,#2202);
#1729=LINE('',#9451,#2203);
#1730=LINE('',#9452,#2204);
#1731=LINE('',#9455,#2205);
#1732=LINE('',#9457,#2206);
#1733=LINE('',#9458,#2207);
#1734=LINE('',#9461,#2208);
#1735=LINE('',#9463,#2209);
#1736=LINE('',#9465,#2210);
#1737=LINE('',#9466,#2211);
#1738=LINE('',#9469,#2212);
#1739=LINE('',#9470,#2213);
#1740=LINE('',#9474,#2214);
#1741=LINE('',#9476,#2215);
#1742=LINE('',#9477,#2216);
#1743=LINE('',#9480,#2217);
#1744=LINE('',#9484,#2218);
#1745=LINE('',#9486,#2219);
#1746=LINE('',#9490,#2220);
#1747=LINE('',#9492,#2221);
#1748=LINE('',#9494,#2222);
#1749=LINE('',#9496,#2223);
#1750=LINE('',#9498,#2224);
#1751=LINE('',#9502,#2225);
#1752=LINE('',#9508,#2226);
#1753=LINE('',#9509,#2227);
#1754=LINE('',#9512,#2228);
#1755=LINE('',#9517,#2229);
#1756=LINE('',#9520,#2230);
#1757=LINE('',#9524,#2231);
#1758=LINE('',#9526,#2232);
#1759=LINE('',#9528,#2233);
#1760=LINE('',#9530,#2234);
#1761=LINE('',#9532,#2235);
#1762=LINE('',#9536,#2236);
#1763=LINE('',#9537,#2237);
#1764=LINE('',#9549,#2238);
#1765=LINE('',#9553,#2239);
#1766=LINE('',#9554,#2240);
#1767=LINE('',#9556,#2241);
#1768=LINE('',#9557,#2242);
#1769=LINE('',#9559,#2243);
#1770=LINE('',#9561,#2244);
#1771=LINE('',#9564,#2245);
#1772=LINE('',#9567,#2246);
#1773=LINE('',#9569,#2247);
#1774=LINE('',#9576,#2248);
#1775=LINE('',#9582,#2249);
#1776=LINE('',#9588,#2250);
#1777=LINE('',#9593,#2251);
#1778=LINE('',#9595,#2252);
#1779=LINE('',#9596,#2253);
#1780=LINE('',#9600,#2254);
#1781=LINE('',#9601,#2255);
#1782=LINE('',#9602,#2256);
#1783=LINE('',#9605,#2257);
#1784=LINE('',#9606,#2258);
#1785=LINE('',#9609,#2259);
#1786=LINE('',#9611,#2260);
#1787=LINE('',#9613,#2261);
#1788=LINE('',#9619,#2262);
#1789=LINE('',#9620,#2263);
#1790=LINE('',#9624,#2264);
#1791=LINE('',#9628,#2265);
#1792=LINE('',#9632,#2266);
#1793=LINE('',#9634,#2267);
#1794=LINE('',#9635,#2268);
#1795=LINE('',#9636,#2269);
#1796=LINE('',#9639,#2270);
#1797=LINE('',#9641,#2271);
#1798=LINE('',#9642,#2272);
#1799=LINE('',#9645,#2273);
#1800=LINE('',#9647,#2274);
#1801=LINE('',#9649,#2275);
#1802=LINE('',#9650,#2276);
#1803=LINE('',#9653,#2277);
#1804=LINE('',#9655,#2278);
#1805=LINE('',#9659,#2279);
#1806=LINE('',#9661,#2280);
#1807=LINE('',#9665,#2281);
#1808=LINE('',#9667,#2282);
#1809=LINE('',#9669,#2283);
#1810=LINE('',#9671,#2284);
#1811=LINE('',#9673,#2285);
#1812=LINE('',#9677,#2286);
#1813=LINE('',#9683,#2287);
#1814=LINE('',#9685,#2288);
#1815=LINE('',#9686,#2289);
#1816=LINE('',#9688,#2290);
#1817=LINE('',#9691,#2291);
#1818=LINE('',#9692,#2292);
#1819=LINE('',#9695,#2293);
#1820=LINE('',#9700,#2294);
#1821=LINE('',#9703,#2295);
#1822=LINE('',#9707,#2296);
#1823=LINE('',#9709,#2297);
#1824=LINE('',#9711,#2298);
#1825=LINE('',#9713,#2299);
#1826=LINE('',#9715,#2300);
#1827=LINE('',#9719,#2301);
#1828=LINE('',#9720,#2302);
#1829=LINE('',#9732,#2303);
#1830=LINE('',#9736,#2304);
#1831=LINE('',#9737,#2305);
#1832=LINE('',#9739,#2306);
#1833=LINE('',#9740,#2307);
#1834=LINE('',#9742,#2308);
#1835=LINE('',#9744,#2309);
#1836=LINE('',#9747,#2310);
#1837=LINE('',#9750,#2311);
#1838=LINE('',#9752,#2312);
#1839=LINE('',#9759,#2313);
#1840=LINE('',#9770,#2314);
#1841=LINE('',#9778,#2315);
#1842=LINE('',#9782,#2316);
#1843=LINE('',#9788,#2317);
#1844=LINE('',#9790,#2318);
#1845=LINE('',#9792,#2319);
#1846=LINE('',#9793,#2320);
#1847=LINE('',#9797,#2321);
#1848=LINE('',#9799,#2322);
#1849=LINE('',#9801,#2323);
#1850=LINE('',#9802,#2324);
#1851=LINE('',#9817,#2325);
#1852=LINE('',#9823,#2326);
#1853=LINE('',#9829,#2327);
#1854=LINE('',#9835,#2328);
#1855=LINE('',#9841,#2329);
#1856=LINE('',#9850,#2330);
#1857=LINE('',#9857,#2331);
#1858=LINE('',#9861,#2332);
#1859=LINE('',#9866,#2333);
#1860=LINE('',#9868,#2334);
#1861=LINE('',#9870,#2335);
#1862=LINE('',#9871,#2336);
#1863=LINE('',#9875,#2337);
#1864=LINE('',#9877,#2338);
#1865=LINE('',#9879,#2339);
#1866=LINE('',#9880,#2340);
#1867=LINE('',#9884,#2341);
#1868=LINE('',#9886,#2342);
#1869=LINE('',#9888,#2343);
#1870=LINE('',#9889,#2344);
#1871=LINE('',#9893,#2345);
#1872=LINE('',#9895,#2346);
#1873=LINE('',#9897,#2347);
#1874=LINE('',#9898,#2348);
#1875=LINE('',#9902,#2349);
#1876=LINE('',#9904,#2350);
#1877=LINE('',#9906,#2351);
#1878=LINE('',#9907,#2352);
#1879=LINE('',#9911,#2353);
#1880=LINE('',#9913,#2354);
#1881=LINE('',#9915,#2355);
#1882=LINE('',#9916,#2356);
#1883=LINE('',#9920,#2357);
#1884=LINE('',#9922,#2358);
#1885=LINE('',#9924,#2359);
#1886=LINE('',#9925,#2360);
#1887=LINE('',#9933,#2361);
#1888=LINE('',#9934,#2362);
#1889=LINE('',#9936,#2363);
#1890=LINE('',#9937,#2364);
#1891=LINE('',#9939,#2365);
#1892=LINE('',#9940,#2366);
#1893=LINE('',#9943,#2367);
#1894=LINE('',#9945,#2368);
#1895=LINE('',#9946,#2369);
#1896=LINE('',#9949,#2370);
#1897=LINE('',#9951,#2371);
#1898=LINE('',#9952,#2372);
#1899=LINE('',#9956,#2373);
#1900=LINE('',#9994,#2374);
#1901=LINE('',#10032,#2375);
#1902=LINE('',#10070,#2376);
#1903=LINE('',#10107,#2377);
#1904=LINE('',#10110,#2378);
#1905=LINE('',#10148,#2379);
#1906=LINE('',#10185,#2380);
#1907=LINE('',#10188,#2381);
#1908=LINE('',#10226,#2382);
#1909=LINE('',#10263,#2383);
#1910=LINE('',#10266,#2384);
#1911=LINE('',#10273,#2385);
#1912=LINE('',#10279,#2386);
#1913=LINE('',#10296,#2387);
#1914=LINE('',#10305,#2388);
#1915=LINE('',#10311,#2389);
#1916=LINE('',#10346,#2390);
#1917=LINE('',#10417,#2391);
#1918=LINE('',#10487,#2392);
#1919=LINE('',#10522,#2393);
#1920=LINE('',#10528,#2394);
#1921=LINE('',#10537,#2395);
#1922=LINE('',#10571,#2396);
#1923=LINE('',#10603,#2397);
#1924=LINE('',#10607,#2398);
#1925=LINE('',#10611,#2399);
#1926=LINE('',#10657,#2400);
#1927=LINE('',#10792,#2401);
#1928=LINE('',#10896,#2402);
#1929=LINE('',#11059,#2403);
#1930=LINE('',#11222,#2404);
#1931=LINE('',#11311,#2405);
#1932=LINE('',#11399,#2406);
#1933=LINE('',#11511,#2407);
#1934=LINE('',#11512,#2408);
#1935=LINE('',#11549,#2409);
#1936=LINE('',#11550,#2410);
#1937=LINE('',#11752,#2411);
#1938=LINE('',#11758,#2412);
#1939=LINE('',#11764,#2413);
#1940=LINE('',#11770,#2414);
#1941=LINE('',#11775,#2415);
#1942=LINE('',#11777,#2416);
#1943=LINE('',#11779,#2417);
#1944=LINE('',#11780,#2418);
#1945=LINE('',#11783,#2419);
#1946=LINE('',#11785,#2420);
#1947=LINE('',#11786,#2421);
#1948=LINE('',#11789,#2422);
#1949=LINE('',#11791,#2423);
#1950=LINE('',#11792,#2424);
#1951=LINE('',#11795,#2425);
#1952=LINE('',#11797,#2426);
#1953=LINE('',#11798,#2427);
#1954=LINE('',#11801,#2428);
#1955=LINE('',#11803,#2429);
#1956=LINE('',#11804,#2430);
#1957=LINE('',#11806,#2431);
#1958=LINE('',#11807,#2432);
#1959=LINE('',#11814,#2433);
#1960=LINE('',#11816,#2434);
#1961=LINE('',#11818,#2435);
#1962=LINE('',#11819,#2436);
#1963=LINE('',#11822,#2437);
#1964=LINE('',#11824,#2438);
#1965=LINE('',#11825,#2439);
#1966=LINE('',#11828,#2440);
#1967=LINE('',#11830,#2441);
#1968=LINE('',#11831,#2442);
#1969=LINE('',#11834,#2443);
#1970=LINE('',#11836,#2444);
#1971=LINE('',#11837,#2445);
#1972=LINE('',#11840,#2446);
#1973=LINE('',#11842,#2447);
#1974=LINE('',#11843,#2448);
#1975=LINE('',#11845,#2449);
#1976=LINE('',#11846,#2450);
#1977=LINE('',#11852,#2451);
#1978=LINE('',#11856,#2452);
#1979=LINE('',#11861,#2453);
#1980=LINE('',#11863,#2454);
#1981=LINE('',#11865,#2455);
#1982=LINE('',#11866,#2456);
#1983=LINE('',#11870,#2457);
#1984=LINE('',#11872,#2458);
#1985=LINE('',#11874,#2459);
#1986=LINE('',#11875,#2460);
#1987=LINE('',#11879,#2461);
#1988=LINE('',#11881,#2462);
#1989=LINE('',#11883,#2463);
#1990=LINE('',#11884,#2464);
#1991=LINE('',#11888,#2465);
#1992=LINE('',#11890,#2466);
#1993=LINE('',#11892,#2467);
#1994=LINE('',#11893,#2468);
#1995=LINE('',#11897,#2469);
#1996=LINE('',#11899,#2470);
#1997=LINE('',#11901,#2471);
#1998=LINE('',#11902,#2472);
#1999=LINE('',#11906,#2473);
#2000=LINE('',#11908,#2474);
#2001=LINE('',#11910,#2475);
#2002=LINE('',#11911,#2476);
#2003=LINE('',#11915,#2477);
#2004=LINE('',#11917,#2478);
#2005=LINE('',#11919,#2479);
#2006=LINE('',#11920,#2480);
#2007=LINE('',#11928,#2481);
#2008=LINE('',#11929,#2482);
#2009=LINE('',#11931,#2483);
#2010=LINE('',#11932,#2484);
#2011=LINE('',#11934,#2485);
#2012=LINE('',#11935,#2486);
#2013=LINE('',#11938,#2487);
#2014=LINE('',#11940,#2488);
#2015=LINE('',#11941,#2489);
#2016=LINE('',#11944,#2490);
#2017=LINE('',#11946,#2491);
#2018=LINE('',#11947,#2492);
#2019=LINE('',#11951,#2493);
#2020=LINE('',#11989,#2494);
#2021=LINE('',#12027,#2495);
#2022=LINE('',#12065,#2496);
#2023=LINE('',#12102,#2497);
#2024=LINE('',#12105,#2498);
#2025=LINE('',#12143,#2499);
#2026=LINE('',#12180,#2500);
#2027=LINE('',#12183,#2501);
#2028=LINE('',#12221,#2502);
#2029=LINE('',#12258,#2503);
#2030=LINE('',#12261,#2504);
#2031=LINE('',#12268,#2505);
#2032=LINE('',#12274,#2506);
#2033=LINE('',#12291,#2507);
#2034=LINE('',#12300,#2508);
#2035=LINE('',#12306,#2509);
#2036=LINE('',#12341,#2510);
#2037=LINE('',#12412,#2511);
#2038=LINE('',#12482,#2512);
#2039=LINE('',#12517,#2513);
#2040=LINE('',#12523,#2514);
#2041=LINE('',#12532,#2515);
#2042=LINE('',#12566,#2516);
#2043=LINE('',#12598,#2517);
#2044=LINE('',#12602,#2518);
#2045=LINE('',#12606,#2519);
#2046=LINE('',#12652,#2520);
#2047=LINE('',#12787,#2521);
#2048=LINE('',#12891,#2522);
#2049=LINE('',#13054,#2523);
#2050=LINE('',#13217,#2524);
#2051=LINE('',#13306,#2525);
#2052=LINE('',#13394,#2526);
#2053=LINE('',#13506,#2527);
#2054=LINE('',#13507,#2528);
#2055=LINE('',#13544,#2529);
#2056=LINE('',#13545,#2530);
#2057=LINE('',#13747,#2531);
#2058=LINE('',#13753,#2532);
#2059=LINE('',#13763,#2533);
#2060=LINE('',#13773,#2534);
#2061=LINE('',#13783,#2535);
#2062=LINE('',#13793,#2536);
#2063=LINE('',#13797,#2537);
#2064=LINE('',#13801,#2538);
#2065=LINE('',#13805,#2539);
#2066=LINE('',#13809,#2540);
#2067=LINE('',#13856,#2541);
#2068=LINE('',#13857,#2542);
#2069=LINE('',#13983,#2543);
#2070=LINE('',#13984,#2544);
#2071=LINE('',#14072,#2545);
#2072=LINE('',#14212,#2546);
#2073=LINE('',#14341,#2547);
#2074=LINE('',#14365,#2548);
#2075=LINE('',#14413,#2549);
#2076=LINE('',#14461,#2550);
#2077=LINE('',#14512,#2551);
#2078=LINE('',#14560,#2552);
#2079=LINE('',#14608,#2553);
#2080=LINE('',#14656,#2554);
#2081=LINE('',#14710,#2555);
#2082=LINE('',#14758,#2556);
#2083=LINE('',#14806,#2557);
#2084=LINE('',#14860,#2558);
#2085=LINE('',#14908,#2559);
#2086=LINE('',#14956,#2560);
#2087=LINE('',#15004,#2561);
#2088=LINE('',#15058,#2562);
#2089=LINE('',#15106,#2563);
#2090=LINE('',#15154,#2564);
#2091=LINE('',#15208,#2565);
#2092=LINE('',#15256,#2566);
#2093=LINE('',#15304,#2567);
#2094=LINE('',#15358,#2568);
#2095=LINE('',#15406,#2569);
#2096=LINE('',#15454,#2570);
#2097=LINE('',#15502,#2571);
#2098=LINE('',#15556,#2572);
#2099=LINE('',#15604,#2573);
#2100=LINE('',#15652,#2574);
#2101=LINE('',#15706,#2575);
#2102=LINE('',#15754,#2576);
#2103=LINE('',#15802,#2577);
#2104=LINE('',#15828,#2578);
#2105=LINE('',#15852,#2579);
#2106=LINE('',#15876,#2580);
#2107=LINE('',#15901,#2581);
#2108=LINE('',#15926,#2582);
#2109=LINE('',#15950,#2583);
#2110=LINE('',#15975,#2584);
#2111=LINE('',#16000,#2585);
#2112=LINE('',#16024,#2586);
#2113=LINE('',#16048,#2587);
#2114=LINE('',#16073,#2588);
#2115=LINE('',#16098,#2589);
#2116=LINE('',#16122,#2590);
#2117=LINE('',#16147,#2591);
#2118=LINE('',#16172,#2592);
#2119=LINE('',#16196,#2593);
#2120=LINE('',#16221,#2594);
#2121=LINE('',#16246,#2595);
#2122=LINE('',#16270,#2596);
#2123=LINE('',#16294,#2597);
#2124=LINE('',#16319,#2598);
#2125=LINE('',#16344,#2599);
#2126=LINE('',#16368,#2600);
#2127=LINE('',#16393,#2601);
#2128=LINE('',#16418,#2602);
#2129=LINE('',#16442,#2603);
#2130=LINE('',#16467,#2604);
#2131=LINE('',#16491,#2605);
#2132=LINE('',#16516,#2606);
#2133=LINE('',#16717,#2607);
#2134=LINE('',#18462,#2608);
#2135=LINE('',#18464,#2609);
#2136=LINE('',#18466,#2610);
#2137=LINE('',#18467,#2611);
#2138=LINE('',#18470,#2612);
#2139=LINE('',#18472,#2613);
#2140=LINE('',#18473,#2614);
#2141=LINE('',#18476,#2615);
#2142=LINE('',#18478,#2616);
#2143=LINE('',#18479,#2617);
#2144=LINE('',#18482,#2618);
#2145=LINE('',#18484,#2619);
#2146=LINE('',#18485,#2620);
#2147=LINE('',#18488,#2621);
#2148=LINE('',#18490,#2622);
#2149=LINE('',#18491,#2623);
#2150=LINE('',#18493,#2624);
#2151=LINE('',#18494,#2625);
#2152=LINE('',#18501,#2626);
#2153=LINE('',#18509,#2627);
#2154=LINE('',#18522,#2628);
#2155=LINE('',#18569,#2629);
#2156=LINE('',#18623,#2630);
#2157=LINE('',#18671,#2631);
#2158=LINE('',#18710,#2632);
#2159=LINE('',#18731,#2633);
#2160=LINE('',#18756,#2634);
#2161=LINE('',#18781,#2635);
#2162=LINE('',#18806,#2636);
#2163=LINE('',#19379,#2637);
#2164=LINE('',#19381,#2638);
#2165=LINE('',#19383,#2639);
#2166=LINE('',#19385,#2640);
#2167=LINE('',#19387,#2641);
#2168=LINE('',#19388,#2642);
#2169=LINE('',#19393,#2643);
#2170=LINE('',#19394,#2644);
#2171=LINE('',#19395,#2645);
#2172=LINE('',#19398,#2646);
#2173=LINE('',#19399,#2647);
#2174=LINE('',#19402,#2648);
#2175=LINE('',#19403,#2649);
#2176=LINE('',#19406,#2650);
#2177=LINE('',#19407,#2651);
#2178=LINE('',#19410,#2652);
#2179=LINE('',#19411,#2653);
#2180=LINE('',#19413,#2654);
#2181=LINE('',#19428,#2655);
#2182=LINE('',#19434,#2656);
#2183=VECTOR('',#7827,0.17);
#2184=VECTOR('',#7834,0.17);
#2185=VECTOR('',#7841,0.41);
#2186=VECTOR('',#7846,1.);
#2187=VECTOR('',#7847,1.);
#2188=VECTOR('',#7848,1.);
#2189=VECTOR('',#7851,1.);
#2190=VECTOR('',#7852,1.);
#2191=VECTOR('',#7853,1.);
#2192=VECTOR('',#7856,1.);
#2193=VECTOR('',#7857,1.);
#2194=VECTOR('',#7860,1.);
#2195=VECTOR('',#7861,1.);
#2196=VECTOR('',#7862,1.);
#2197=VECTOR('',#7863,1.);
#2198=VECTOR('',#7864,1.);
#2199=VECTOR('',#7869,1.);
#2200=VECTOR('',#7870,1.);
#2201=VECTOR('',#7877,1.);
#2202=VECTOR('',#7882,1.);
#2203=VECTOR('',#7885,1.);
#2204=VECTOR('',#7886,1.);
#2205=VECTOR('',#7889,1.);
#2206=VECTOR('',#7890,1.);
#2207=VECTOR('',#7891,1.);
#2208=VECTOR('',#7894,1.);
#2209=VECTOR('',#7895,1.);
#2210=VECTOR('',#7896,1.);
#2211=VECTOR('',#7897,1.);
#2212=VECTOR('',#7900,1.);
#2213=VECTOR('',#7901,1.);
#2214=VECTOR('',#7906,1.);
#2215=VECTOR('',#7907,1.);
#2216=VECTOR('',#7908,1.);
#2217=VECTOR('',#7911,1.);
#2218=VECTOR('',#7914,1.);
#2219=VECTOR('',#7915,1.);
#2220=VECTOR('',#7918,1.);
#2221=VECTOR('',#7919,1.);
#2222=VECTOR('',#7920,1.);
#2223=VECTOR('',#7921,1.);
#2224=VECTOR('',#7922,1.);
#2225=VECTOR('',#7925,1.);
#2226=VECTOR('',#7932,1.);
#2227=VECTOR('',#7933,1.);
#2228=VECTOR('',#7936,1.);
#2229=VECTOR('',#7943,1.);
#2230=VECTOR('',#7946,1.);
#2231=VECTOR('',#7949,1.);
#2232=VECTOR('',#7950,1.);
#2233=VECTOR('',#7951,1.);
#2234=VECTOR('',#7952,1.);
#2235=VECTOR('',#7953,1.);
#2236=VECTOR('',#7956,1.);
#2237=VECTOR('',#7957,1.);
#2238=VECTOR('',#7972,1.1);
#2239=VECTOR('',#7979,1.);
#2240=VECTOR('',#7980,1.);
#2241=VECTOR('',#7983,1.);
#2242=VECTOR('',#7984,1.);
#2243=VECTOR('',#7987,1.);
#2244=VECTOR('',#7990,1.);
#2245=VECTOR('',#7995,1.);
#2246=VECTOR('',#8000,1.);
#2247=VECTOR('',#8003,1.);
#2248=VECTOR('',#8012,0.17);
#2249=VECTOR('',#8019,0.17);
#2250=VECTOR('',#8026,0.41);
#2251=VECTOR('',#8031,1.);
#2252=VECTOR('',#8032,1.);
#2253=VECTOR('',#8033,1.);
#2254=VECTOR('',#8036,1.);
#2255=VECTOR('',#8037,1.);
#2256=VECTOR('',#8038,1.);
#2257=VECTOR('',#8041,1.);
#2258=VECTOR('',#8042,1.);
#2259=VECTOR('',#8045,1.);
#2260=VECTOR('',#8046,1.);
#2261=VECTOR('',#8047,1.);
#2262=VECTOR('',#8056,1.);
#2263=VECTOR('',#8057,1.);
#2264=VECTOR('',#8062,1.);
#2265=VECTOR('',#8067,1.);
#2266=VECTOR('',#8070,1.);
#2267=VECTOR('',#8071,1.);
#2268=VECTOR('',#8072,1.);
#2269=VECTOR('',#8073,1.);
#2270=VECTOR('',#8076,1.);
#2271=VECTOR('',#8077,1.);
#2272=VECTOR('',#8078,1.);
#2273=VECTOR('',#8081,1.);
#2274=VECTOR('',#8082,1.);
#2275=VECTOR('',#8083,1.);
#2276=VECTOR('',#8084,1.);
#2277=VECTOR('',#8087,1.);
#2278=VECTOR('',#8088,1.);
#2279=VECTOR('',#8091,1.);
#2280=VECTOR('',#8092,1.);
#2281=VECTOR('',#8095,1.);
#2282=VECTOR('',#8096,1.);
#2283=VECTOR('',#8097,1.);
#2284=VECTOR('',#8098,1.);
#2285=VECTOR('',#8099,1.);
#2286=VECTOR('',#8102,1.);
#2287=VECTOR('',#8109,1.);
#2288=VECTOR('',#8110,1.);
#2289=VECTOR('',#8111,1.);
#2290=VECTOR('',#8114,1.);
#2291=VECTOR('',#8117,1.);
#2292=VECTOR('',#8118,1.);
#2293=VECTOR('',#8121,1.);
#2294=VECTOR('',#8128,1.);
#2295=VECTOR('',#8131,1.);
#2296=VECTOR('',#8134,1.);
#2297=VECTOR('',#8135,1.);
#2298=VECTOR('',#8136,1.);
#2299=VECTOR('',#8137,1.);
#2300=VECTOR('',#8138,1.);
#2301=VECTOR('',#8141,1.);
#2302=VECTOR('',#8142,1.);
#2303=VECTOR('',#8157,1.1);
#2304=VECTOR('',#8164,1.);
#2305=VECTOR('',#8165,1.);
#2306=VECTOR('',#8168,1.);
#2307=VECTOR('',#8169,1.);
#2308=VECTOR('',#8172,1.);
#2309=VECTOR('',#8175,1.);
#2310=VECTOR('',#8180,1.);
#2311=VECTOR('',#8185,1.);
#2312=VECTOR('',#8188,1.);
#2313=VECTOR('',#8197,0.3);
#2314=VECTOR('',#8212,0.4);
#2315=VECTOR('',#8221,0.6);
#2316=VECTOR('',#8228,0.4);
#2317=VECTOR('',#8235,1.);
#2318=VECTOR('',#8236,1.);
#2319=VECTOR('',#8237,1.);
#2320=VECTOR('',#8238,1.);
#2321=VECTOR('',#8241,1.);
#2322=VECTOR('',#8242,1.);
#2323=VECTOR('',#8243,1.);
#2324=VECTOR('',#8244,1.);
#2325=VECTOR('',#8269,0.15);
#2326=VECTOR('',#8276,0.15);
#2327=VECTOR('',#8283,0.15);
#2328=VECTOR('',#8290,0.15);
#2329=VECTOR('',#8297,0.3);
#2330=VECTOR('',#8308,0.3);
#2331=VECTOR('',#8317,0.17);
#2332=VECTOR('',#8322,0.17);
#2333=VECTOR('',#8327,1.);
#2334=VECTOR('',#8328,1.);
#2335=VECTOR('',#8329,1.);
#2336=VECTOR('',#8330,1.);
#2337=VECTOR('',#8333,1.);
#2338=VECTOR('',#8334,1.);
#2339=VECTOR('',#8335,1.);
#2340=VECTOR('',#8336,1.);
#2341=VECTOR('',#8339,1.);
#2342=VECTOR('',#8340,1.);
#2343=VECTOR('',#8341,1.);
#2344=VECTOR('',#8342,1.);
#2345=VECTOR('',#8345,1.);
#2346=VECTOR('',#8346,1.);
#2347=VECTOR('',#8347,1.);
#2348=VECTOR('',#8348,1.);
#2349=VECTOR('',#8351,1.);
#2350=VECTOR('',#8352,1.);
#2351=VECTOR('',#8353,1.);
#2352=VECTOR('',#8354,1.);
#2353=VECTOR('',#8357,1.);
#2354=VECTOR('',#8358,1.);
#2355=VECTOR('',#8359,1.);
#2356=VECTOR('',#8360,1.);
#2357=VECTOR('',#8363,1.);
#2358=VECTOR('',#8364,1.);
#2359=VECTOR('',#8365,1.);
#2360=VECTOR('',#8366,1.);
#2361=VECTOR('',#8377,1.);
#2362=VECTOR('',#8378,1.);
#2363=VECTOR('',#8381,1.);
#2364=VECTOR('',#8382,1.);
#2365=VECTOR('',#8385,1.);
#2366=VECTOR('',#8386,1.);
#2367=VECTOR('',#8389,1.);
#2368=VECTOR('',#8390,1.);
#2369=VECTOR('',#8391,1.);
#2370=VECTOR('',#8394,1.);
#2371=VECTOR('',#8395,1.);
#2372=VECTOR('',#8396,1.);
#2373=VECTOR('',#8399,1.);
#2374=VECTOR('',#8400,1.);
#2375=VECTOR('',#8403,1.);
#2376=VECTOR('',#8404,1.);
#2377=VECTOR('',#8405,1.);
#2378=VECTOR('',#8408,1.);
#2379=VECTOR('',#8409,1.);
#2380=VECTOR('',#8410,1.);
#2381=VECTOR('',#8413,1.);
#2382=VECTOR('',#8414,1.);
#2383=VECTOR('',#8415,1.);
#2384=VECTOR('',#8418,1.);
#2385=VECTOR('',#8419,1.);
#2386=VECTOR('',#8420,1.);
#2387=VECTOR('',#8423,1.);
#2388=VECTOR('',#8424,1.);
#2389=VECTOR('',#8425,1.);
#2390=VECTOR('',#8426,1.);
#2391=VECTOR('',#8427,1.);
#2392=VECTOR('',#8428,1.);
#2393=VECTOR('',#8429,1.);
#2394=VECTOR('',#8430,1.);
#2395=VECTOR('',#8431,1.);
#2396=VECTOR('',#8432,1.);
#2397=VECTOR('',#8433,1.);
#2398=VECTOR('',#8438,0.4);
#2399=VECTOR('',#8443,0.4);
#2400=VECTOR('',#8446,1.);
#2401=VECTOR('',#8453,1.);
#2402=VECTOR('',#8456,1.);
#2403=VECTOR('',#8461,1.);
#2404=VECTOR('',#8466,1.);
#2405=VECTOR('',#8471,1.);
#2406=VECTOR('',#8504,1.);
#2407=VECTOR('',#8533,1.);
#2408=VECTOR('',#8534,1.);
#2409=VECTOR('',#8545,1.);
#2410=VECTOR('',#8546,1.);
#2411=VECTOR('',#8559,0.15);
#2412=VECTOR('',#8566,0.15);
#2413=VECTOR('',#8573,0.15);
#2414=VECTOR('',#8580,0.15);
#2415=VECTOR('',#8585,1.);
#2416=VECTOR('',#8586,1.);
#2417=VECTOR('',#8587,1.);
#2418=VECTOR('',#8588,1.);
#2419=VECTOR('',#8591,1.);
#2420=VECTOR('',#8592,1.);
#2421=VECTOR('',#8593,1.);
#2422=VECTOR('',#8596,1.);
#2423=VECTOR('',#8597,1.);
#2424=VECTOR('',#8598,1.);
#2425=VECTOR('',#8601,1.);
#2426=VECTOR('',#8602,1.);
#2427=VECTOR('',#8603,1.);
#2428=VECTOR('',#8606,1.);
#2429=VECTOR('',#8607,1.);
#2430=VECTOR('',#8608,1.);
#2431=VECTOR('',#8611,1.);
#2432=VECTOR('',#8612,1.);
#2433=VECTOR('',#8619,1.);
#2434=VECTOR('',#8620,1.);
#2435=VECTOR('',#8621,1.);
#2436=VECTOR('',#8622,1.);
#2437=VECTOR('',#8625,1.);
#2438=VECTOR('',#8626,1.);
#2439=VECTOR('',#8627,1.);
#2440=VECTOR('',#8630,1.);
#2441=VECTOR('',#8631,1.);
#2442=VECTOR('',#8632,1.);
#2443=VECTOR('',#8635,1.);
#2444=VECTOR('',#8636,1.);
#2445=VECTOR('',#8637,1.);
#2446=VECTOR('',#8640,1.);
#2447=VECTOR('',#8641,1.);
#2448=VECTOR('',#8642,1.);
#2449=VECTOR('',#8645,1.);
#2450=VECTOR('',#8646,1.);
#2451=VECTOR('',#8653,0.17);
#2452=VECTOR('',#8658,0.17);
#2453=VECTOR('',#8663,1.);
#2454=VECTOR('',#8664,1.);
#2455=VECTOR('',#8665,1.);
#2456=VECTOR('',#8666,1.);
#2457=VECTOR('',#8669,1.);
#2458=VECTOR('',#8670,1.);
#2459=VECTOR('',#8671,1.);
#2460=VECTOR('',#8672,1.);
#2461=VECTOR('',#8675,1.);
#2462=VECTOR('',#8676,1.);
#2463=VECTOR('',#8677,1.);
#2464=VECTOR('',#8678,1.);
#2465=VECTOR('',#8681,1.);
#2466=VECTOR('',#8682,1.);
#2467=VECTOR('',#8683,1.);
#2468=VECTOR('',#8684,1.);
#2469=VECTOR('',#8687,1.);
#2470=VECTOR('',#8688,1.);
#2471=VECTOR('',#8689,1.);
#2472=VECTOR('',#8690,1.);
#2473=VECTOR('',#8693,1.);
#2474=VECTOR('',#8694,1.);
#2475=VECTOR('',#8695,1.);
#2476=VECTOR('',#8696,1.);
#2477=VECTOR('',#8699,1.);
#2478=VECTOR('',#8700,1.);
#2479=VECTOR('',#8701,1.);
#2480=VECTOR('',#8702,1.);
#2481=VECTOR('',#8713,1.);
#2482=VECTOR('',#8714,1.);
#2483=VECTOR('',#8717,1.);
#2484=VECTOR('',#8718,1.);
#2485=VECTOR('',#8721,1.);
#2486=VECTOR('',#8722,1.);
#2487=VECTOR('',#8725,1.);
#2488=VECTOR('',#8726,1.);
#2489=VECTOR('',#8727,1.);
#2490=VECTOR('',#8730,1.);
#2491=VECTOR('',#8731,1.);
#2492=VECTOR('',#8732,1.);
#2493=VECTOR('',#8735,1.);
#2494=VECTOR('',#8736,1.);
#2495=VECTOR('',#8739,1.);
#2496=VECTOR('',#8740,1.);
#2497=VECTOR('',#8741,1.);
#2498=VECTOR('',#8744,1.);
#2499=VECTOR('',#8745,1.);
#2500=VECTOR('',#8746,1.);
#2501=VECTOR('',#8749,1.);
#2502=VECTOR('',#8750,1.);
#2503=VECTOR('',#8751,1.);
#2504=VECTOR('',#8754,1.);
#2505=VECTOR('',#8755,1.);
#2506=VECTOR('',#8756,1.);
#2507=VECTOR('',#8759,1.);
#2508=VECTOR('',#8760,1.);
#2509=VECTOR('',#8761,1.);
#2510=VECTOR('',#8762,1.);
#2511=VECTOR('',#8763,1.);
#2512=VECTOR('',#8764,1.);
#2513=VECTOR('',#8765,1.);
#2514=VECTOR('',#8766,1.);
#2515=VECTOR('',#8767,1.);
#2516=VECTOR('',#8768,1.);
#2517=VECTOR('',#8769,1.);
#2518=VECTOR('',#8774,0.4);
#2519=VECTOR('',#8779,0.4);
#2520=VECTOR('',#8782,1.);
#2521=VECTOR('',#8789,1.);
#2522=VECTOR('',#8792,1.);
#2523=VECTOR('',#8797,1.);
#2524=VECTOR('',#8802,1.);
#2525=VECTOR('',#8807,1.);
#2526=VECTOR('',#8840,1.);
#2527=VECTOR('',#8869,1.);
#2528=VECTOR('',#8870,1.);
#2529=VECTOR('',#8881,1.);
#2530=VECTOR('',#8882,1.);
#2531=VECTOR('',#8895,0.35);
#2532=VECTOR('',#8902,0.35);
#2533=VECTOR('',#8915,0.25);
#2534=VECTOR('',#8928,0.25);
#2535=VECTOR('',#8941,0.25);
#2536=VECTOR('',#8954,0.25);
#2537=VECTOR('',#8959,0.15);
#2538=VECTOR('',#8964,0.15);
#2539=VECTOR('',#8969,0.15);
#2540=VECTOR('',#8974,0.15);
#2541=VECTOR('',#8985,1.);
#2542=VECTOR('',#8986,1.);
#2543=VECTOR('',#8997,1.);
#2544=VECTOR('',#8998,1.);
#2545=VECTOR('',#9003,1.);
#2546=VECTOR('',#9008,1.);
#2547=VECTOR('',#9015,0.15);
#2548=VECTOR('',#9020,0.15);
#2549=VECTOR('',#9023,0.15);
#2550=VECTOR('',#9026,0.15);
#2551=VECTOR('',#9029,0.15);
#2552=VECTOR('',#9032,0.15);
#2553=VECTOR('',#9035,0.15);
#2554=VECTOR('',#9038,0.15);
#2555=VECTOR('',#9041,0.15);
#2556=VECTOR('',#9044,0.15);
#2557=VECTOR('',#9047,0.15);
#2558=VECTOR('',#9050,0.15);
#2559=VECTOR('',#9053,0.15);
#2560=VECTOR('',#9056,0.15);
#2561=VECTOR('',#9059,0.15);
#2562=VECTOR('',#9062,0.15);
#2563=VECTOR('',#9065,0.15);
#2564=VECTOR('',#9068,0.15);
#2565=VECTOR('',#9071,0.15);
#2566=VECTOR('',#9074,0.15);
#2567=VECTOR('',#9077,0.15);
#2568=VECTOR('',#9080,0.15);
#2569=VECTOR('',#9083,0.15);
#2570=VECTOR('',#9086,0.15);
#2571=VECTOR('',#9089,0.15);
#2572=VECTOR('',#9092,0.15);
#2573=VECTOR('',#9095,0.15);
#2574=VECTOR('',#9098,0.15);
#2575=VECTOR('',#9101,0.15);
#2576=VECTOR('',#9104,0.15);
#2577=VECTOR('',#9107,0.117775);
#2578=VECTOR('',#9112,0.117775);
#2579=VECTOR('',#9115,0.117775);
#2580=VECTOR('',#9118,0.117775);
#2581=VECTOR('',#9121,0.117775);
#2582=VECTOR('',#9124,0.117775);
#2583=VECTOR('',#9127,0.117775);
#2584=VECTOR('',#9130,0.117775);
#2585=VECTOR('',#9133,0.117775);
#2586=VECTOR('',#9136,0.117775);
#2587=VECTOR('',#9139,0.117775);
#2588=VECTOR('',#9142,0.117775);
#2589=VECTOR('',#9145,0.117775);
#2590=VECTOR('',#9148,0.117775);
#2591=VECTOR('',#9151,0.117775);
#2592=VECTOR('',#9154,0.117775);
#2593=VECTOR('',#9157,0.117775);
#2594=VECTOR('',#9160,0.117775);
#2595=VECTOR('',#9163,0.117775);
#2596=VECTOR('',#9166,0.117775);
#2597=VECTOR('',#9169,0.117775);
#2598=VECTOR('',#9172,0.117775);
#2599=VECTOR('',#9175,0.117775);
#2600=VECTOR('',#9178,0.117775);
#2601=VECTOR('',#9181,0.117775);
#2602=VECTOR('',#9184,0.117775);
#2603=VECTOR('',#9187,0.117775);
#2604=VECTOR('',#9190,0.117775);
#2605=VECTOR('',#9193,0.117775);
#2606=VECTOR('',#9196,0.117775);
#2607=VECTOR('',#9201,0.1);
#2608=VECTOR('',#9212,1.);
#2609=VECTOR('',#9213,1.);
#2610=VECTOR('',#9214,1.);
#2611=VECTOR('',#9215,1.);
#2612=VECTOR('',#9218,1.);
#2613=VECTOR('',#9219,1.);
#2614=VECTOR('',#9220,1.);
#2615=VECTOR('',#9223,1.);
#2616=VECTOR('',#9224,1.);
#2617=VECTOR('',#9225,1.);
#2618=VECTOR('',#9228,1.);
#2619=VECTOR('',#9229,1.);
#2620=VECTOR('',#9230,1.);
#2621=VECTOR('',#9233,1.);
#2622=VECTOR('',#9234,1.);
#2623=VECTOR('',#9235,1.);
#2624=VECTOR('',#9238,1.);
#2625=VECTOR('',#9239,1.);
#2626=VECTOR('',#9248,0.275);
#2627=VECTOR('',#9259,0.15);
#2628=VECTOR('',#9264,0.15);
#2629=VECTOR('',#9269,0.15);
#2630=VECTOR('',#9272,0.15);
#2631=VECTOR('',#9275,0.15);
#2632=VECTOR('',#9280,0.1543);
#2633=VECTOR('',#9285,0.1543);
#2634=VECTOR('',#9288,0.1543);
#2635=VECTOR('',#9291,0.1543);
#2636=VECTOR('',#9294,0.1543);
#2637=VECTOR('',#9301,1.);
#2638=VECTOR('',#9302,1.);
#2639=VECTOR('',#9303,1.);
#2640=VECTOR('',#9304,1.);
#2641=VECTOR('',#9305,1.);
#2642=VECTOR('',#9306,1.);
#2643=VECTOR('',#9311,1.);
#2644=VECTOR('',#9312,1.);
#2645=VECTOR('',#9313,1.);
#2646=VECTOR('',#9316,1.);
#2647=VECTOR('',#9317,1.);
#2648=VECTOR('',#9320,1.);
#2649=VECTOR('',#9321,1.);
#2650=VECTOR('',#9324,1.);
#2651=VECTOR('',#9325,1.);
#2652=VECTOR('',#9328,1.);
#2653=VECTOR('',#9329,1.);
#2654=VECTOR('',#9332,1.);
#2655=VECTOR('',#9357,0.41);
#2656=VECTOR('',#9364,0.6);
#2657=CIRCLE('',#7275,0.17);
#2658=CIRCLE('',#7276,0.17);
#2659=CIRCLE('',#7278,0.17);
#2660=CIRCLE('',#7279,0.17);
#2661=CIRCLE('',#7281,0.41);
#2662=CIRCLE('',#7282,0.41);
#2663=CIRCLE('',#7287,17.7082646568653);
#2664=CIRCLE('',#7290,0.2);
#2665=CIRCLE('',#7291,0.2);
#2666=CIRCLE('',#7293,17.7082646568653);
#2667=CIRCLE('',#7301,1.4);
#2668=CIRCLE('',#7302,1.7);
#2669=CIRCLE('',#7303,1.7);
#2670=CIRCLE('',#7304,1.4);
#2671=CIRCLE('',#7305,1.2);
#2672=CIRCLE('',#7308,1.4);
#2673=CIRCLE('',#7310,1.4);
#2674=CIRCLE('',#7312,1.7);
#2675=CIRCLE('',#7313,1.7);
#2676=CIRCLE('',#7314,1.2);
#2677=CIRCLE('',#7316,0.1);
#2678=CIRCLE('',#7317,1.1);
#2679=CIRCLE('',#7319,1.1);
#2680=CIRCLE('',#7320,1.1);
#2681=CIRCLE('',#7322,0.1);
#2682=CIRCLE('',#7335,0.17);
#2683=CIRCLE('',#7336,0.17);
#2684=CIRCLE('',#7338,0.17);
#2685=CIRCLE('',#7339,0.17);
#2686=CIRCLE('',#7341,0.41);
#2687=CIRCLE('',#7342,0.41);
#2688=CIRCLE('',#7347,17.7082646568653);
#2689=CIRCLE('',#7349,0.2);
#2690=CIRCLE('',#7352,0.2);
#2691=CIRCLE('',#7354,17.7082646568653);
#2692=CIRCLE('',#7359,1.4);
#2693=CIRCLE('',#7360,1.7);
#2694=CIRCLE('',#7361,1.7);
#2695=CIRCLE('',#7362,1.4);
#2696=CIRCLE('',#7363,1.2);
#2697=CIRCLE('',#7368,1.4);
#2698=CIRCLE('',#7370,1.4);
#2699=CIRCLE('',#7372,1.7);
#2700=CIRCLE('',#7373,1.7);
#2701=CIRCLE('',#7374,1.2);
#2702=CIRCLE('',#7376,0.1);
#2703=CIRCLE('',#7377,1.1);
#2704=CIRCLE('',#7379,1.1);
#2705=CIRCLE('',#7380,1.1);
#2706=CIRCLE('',#7382,0.1);
#2707=CIRCLE('',#7395,0.3);
#2708=CIRCLE('',#7396,0.3);
#2709=CIRCLE('',#7398,0.4);
#2710=CIRCLE('',#7400,0.4);
#2711=CIRCLE('',#7402,0.4);
#2712=CIRCLE('',#7404,0.6);
#2713=CIRCLE('',#7405,0.4);
#2714=CIRCLE('',#7407,0.6);
#2715=CIRCLE('',#7415,0.6);
#2716=CIRCLE('',#7416,0.3);
#2717=CIRCLE('',#7418,0.3);
#2718=CIRCLE('',#7420,0.6);
#2719=CIRCLE('',#7425,0.15);
#2720=CIRCLE('',#7426,0.15);
#2721=CIRCLE('',#7428,0.15);
#2722=CIRCLE('',#7429,0.15);
#2723=CIRCLE('',#7431,0.15);
#2724=CIRCLE('',#7432,0.15);
#2725=CIRCLE('',#7434,0.15);
#2726=CIRCLE('',#7435,0.15);
#2727=CIRCLE('',#7437,0.3);
#2728=CIRCLE('',#7438,0.3);
#2729=CIRCLE('',#7440,0.17);
#2730=CIRCLE('',#7442,0.3);
#2731=CIRCLE('',#7443,0.3);
#2732=CIRCLE('',#7445,0.17);
#2733=CIRCLE('',#7447,0.17);
#2734=CIRCLE('',#7449,0.17);
#2735=CIRCLE('',#7458,0.4);
#2736=CIRCLE('',#7460,0.4);
#2737=CIRCLE('',#7473,0.4);
#2738=CIRCLE('',#7475,0.4);
#2739=CIRCLE('',#7477,0.1);
#2740=CIRCLE('',#7485,0.0999999999999994);
#2741=CIRCLE('',#7487,0.0999999999999999);
#2742=CIRCLE('',#7489,0.1);
#2743=CIRCLE('',#7490,0.1);
#2744=CIRCLE('',#7492,0.100000000000001);
#2745=CIRCLE('',#7493,0.100000000000001);
#2746=CIRCLE('',#7494,0.100000000000002);
#2747=CIRCLE('',#7496,0.0999999999999995);
#2748=CIRCLE('',#7497,0.0999999999999991);
#2749=CIRCLE('',#7500,0.100000000000001);
#2750=CIRCLE('',#7501,0.1);
#2751=CIRCLE('',#7505,0.3);
#2752=CIRCLE('',#7506,0.3);
#2753=CIRCLE('',#7507,0.3);
#2754=CIRCLE('',#7509,0.3);
#2755=CIRCLE('',#7510,0.300000000000002);
#2756=CIRCLE('',#7511,0.3);
#2757=CIRCLE('',#7513,0.3);
#2758=CIRCLE('',#7514,0.299999999999999);
#2759=CIRCLE('',#7515,0.3);
#2760=CIRCLE('',#7518,0.300000000000001);
#2761=CIRCLE('',#7519,0.3);
#2762=CIRCLE('',#7520,0.3);
#2763=CIRCLE('',#7527,0.15);
#2764=CIRCLE('',#7528,0.15);
#2765=CIRCLE('',#7530,0.15);
#2766=CIRCLE('',#7531,0.15);
#2767=CIRCLE('',#7533,0.15);
#2768=CIRCLE('',#7534,0.15);
#2769=CIRCLE('',#7536,0.15);
#2770=CIRCLE('',#7537,0.15);
#2771=CIRCLE('',#7545,0.17);
#2772=CIRCLE('',#7553,0.17);
#2773=CIRCLE('',#7555,0.17);
#2774=CIRCLE('',#7557,0.17);
#2775=CIRCLE('',#7566,0.4);
#2776=CIRCLE('',#7568,0.4);
#2777=CIRCLE('',#7581,0.4);
#2778=CIRCLE('',#7583,0.4);
#2779=CIRCLE('',#7585,0.1);
#2780=CIRCLE('',#7593,0.0999999999999994);
#2781=CIRCLE('',#7595,0.0999999999999999);
#2782=CIRCLE('',#7597,0.1);
#2783=CIRCLE('',#7598,0.1);
#2784=CIRCLE('',#7600,0.100000000000001);
#2785=CIRCLE('',#7601,0.100000000000001);
#2786=CIRCLE('',#7602,0.100000000000002);
#2787=CIRCLE('',#7604,0.0999999999999995);
#2788=CIRCLE('',#7605,0.0999999999999991);
#2789=CIRCLE('',#7608,0.100000000000001);
#2790=CIRCLE('',#7609,0.1);
#2791=CIRCLE('',#7613,0.3);
#2792=CIRCLE('',#7614,0.3);
#2793=CIRCLE('',#7615,0.3);
#2794=CIRCLE('',#7617,0.3);
#2795=CIRCLE('',#7618,0.300000000000002);
#2796=CIRCLE('',#7619,0.3);
#2797=CIRCLE('',#7621,0.3);
#2798=CIRCLE('',#7622,0.299999999999999);
#2799=CIRCLE('',#7623,0.3);
#2800=CIRCLE('',#7626,0.300000000000001);
#2801=CIRCLE('',#7627,0.3);
#2802=CIRCLE('',#7628,0.3);
#2803=CIRCLE('',#7635,0.35);
#2804=CIRCLE('',#7636,0.35);
#2805=CIRCLE('',#7638,0.35);
#2806=CIRCLE('',#7639,0.35);
#2807=CIRCLE('',#7641,0.25);
#2808=CIRCLE('',#7642,0.15);
#2809=CIRCLE('',#7644,0.25);
#2810=CIRCLE('',#7647,0.25);
#2811=CIRCLE('',#7648,0.15);
#2812=CIRCLE('',#7650,0.25);
#2813=CIRCLE('',#7653,0.25);
#2814=CIRCLE('',#7654,0.15);
#2815=CIRCLE('',#7656,0.25);
#2816=CIRCLE('',#7659,0.25);
#2817=CIRCLE('',#7660,0.15);
#2818=CIRCLE('',#7662,0.25);
#2819=CIRCLE('',#7665,0.15);
#2820=CIRCLE('',#7667,0.15);
#2821=CIRCLE('',#7669,0.15);
#2822=CIRCLE('',#7671,0.15);
#2823=CIRCLE('',#7672,0.0800000000000001);
#2824=CIRCLE('',#7673,0.0799999999999999);
#2825=CIRCLE('',#7675,0.0800000000000001);
#2826=CIRCLE('',#7676,0.0799999999999998);
#2827=CIRCLE('',#7677,0.0800000000000001);
#2828=CIRCLE('',#7678,0.0800000000000001);
#2829=CIRCLE('',#7680,0.0800000000000001);
#2830=CIRCLE('',#7681,0.0799999999999998);
#2831=CIRCLE('',#7688,0.14635);
#2832=CIRCLE('',#7719,0.117775);
#2833=CIRCLE('',#7750,0.14635);
#2834=CIRCLE('',#7751,0.05);
#2835=CIRCLE('',#7753,0.117775);
#2836=CIRCLE('',#7763,0.275);
#2837=CIRCLE('',#7765,0.275);
#2838=CIRCLE('',#7770,0.12645);
#2839=CIRCLE('',#7772,0.12645);
#2840=CIRCLE('',#7776,0.12645);
#2841=CIRCLE('',#7778,0.1543);
#2842=CIRCLE('',#7783,0.1543);
#2843=CIRCLE('',#7804,0.41);
#2844=CIRCLE('',#7805,0.41);
#2845=CIRCLE('',#7807,0.6);
#2846=CIRCLE('',#7808,0.6);
#2847=VERTEX_POINT('',#9390);
#2848=VERTEX_POINT('',#9392);
#2849=VERTEX_POINT('',#9396);
#2850=VERTEX_POINT('',#9398);
#2851=VERTEX_POINT('',#9402);
#2852=VERTEX_POINT('',#9404);
#2853=VERTEX_POINT('',#9408);
#2854=VERTEX_POINT('',#9409);
#2855=VERTEX_POINT('',#9411);
#2856=VERTEX_POINT('',#9415);
#2857=VERTEX_POINT('',#9416);
#2858=VERTEX_POINT('',#9421);
#2859=VERTEX_POINT('',#9425);
#2860=VERTEX_POINT('',#9427);
#2861=VERTEX_POINT('',#9429);
#2862=VERTEX_POINT('',#9431);
#2863=VERTEX_POINT('',#9433);
#2864=VERTEX_POINT('',#9437);
#2865=VERTEX_POINT('',#9441);
#2866=VERTEX_POINT('',#9446);
#2867=VERTEX_POINT('',#9450);
#2868=VERTEX_POINT('',#9454);
#2869=VERTEX_POINT('',#9456);
#2870=VERTEX_POINT('',#9460);
#2871=VERTEX_POINT('',#9462);
#2872=VERTEX_POINT('',#9464);
#2873=VERTEX_POINT('',#9468);
#2874=VERTEX_POINT('',#9473);
#2875=VERTEX_POINT('',#9475);
#2876=VERTEX_POINT('',#9479);
#2877=VERTEX_POINT('',#9481);
#2878=VERTEX_POINT('',#9483);
#2879=VERTEX_POINT('',#9485);
#2880=VERTEX_POINT('',#9487);
#2881=VERTEX_POINT('',#9489);
#2882=VERTEX_POINT('',#9491);
#2883=VERTEX_POINT('',#9493);
#2884=VERTEX_POINT('',#9495);
#2885=VERTEX_POINT('',#9497);
#2886=VERTEX_POINT('',#9499);
#2887=VERTEX_POINT('',#9501);
#2888=VERTEX_POINT('',#9504);
#2889=VERTEX_POINT('',#9507);
#2890=VERTEX_POINT('',#9511);
#2891=VERTEX_POINT('',#9515);
#2892=VERTEX_POINT('',#9519);
#2893=VERTEX_POINT('',#9521);
#2894=VERTEX_POINT('',#9523);
#2895=VERTEX_POINT('',#9525);
#2896=VERTEX_POINT('',#9527);
#2897=VERTEX_POINT('',#9529);
#2898=VERTEX_POINT('',#9531);
#2899=VERTEX_POINT('',#9533);
#2900=VERTEX_POINT('',#9535);
#2901=VERTEX_POINT('',#9538);
#2902=VERTEX_POINT('',#9541);
#2903=VERTEX_POINT('',#9545);
#2904=VERTEX_POINT('',#9546);
#2905=VERTEX_POINT('',#9573);
#2906=VERTEX_POINT('',#9575);
#2907=VERTEX_POINT('',#9579);
#2908=VERTEX_POINT('',#9581);
#2909=VERTEX_POINT('',#9585);
#2910=VERTEX_POINT('',#9587);
#2911=VERTEX_POINT('',#9591);
#2912=VERTEX_POINT('',#9592);
#2913=VERTEX_POINT('',#9594);
#2914=VERTEX_POINT('',#9598);
#2915=VERTEX_POINT('',#9599);
#2916=VERTEX_POINT('',#9604);
#2917=VERTEX_POINT('',#9608);
#2918=VERTEX_POINT('',#9610);
#2919=VERTEX_POINT('',#9612);
#2920=VERTEX_POINT('',#9618);
#2921=VERTEX_POINT('',#9622);
#2922=VERTEX_POINT('',#9626);
#2923=VERTEX_POINT('',#9630);
#2924=VERTEX_POINT('',#9631);
#2925=VERTEX_POINT('',#9633);
#2926=VERTEX_POINT('',#9638);
#2927=VERTEX_POINT('',#9640);
#2928=VERTEX_POINT('',#9644);
#2929=VERTEX_POINT('',#9646);
#2930=VERTEX_POINT('',#9648);
#2931=VERTEX_POINT('',#9652);
#2932=VERTEX_POINT('',#9654);
#2933=VERTEX_POINT('',#9656);
#2934=VERTEX_POINT('',#9658);
#2935=VERTEX_POINT('',#9660);
#2936=VERTEX_POINT('',#9662);
#2937=VERTEX_POINT('',#9664);
#2938=VERTEX_POINT('',#9666);
#2939=VERTEX_POINT('',#9668);
#2940=VERTEX_POINT('',#9670);
#2941=VERTEX_POINT('',#9672);
#2942=VERTEX_POINT('',#9674);
#2943=VERTEX_POINT('',#9676);
#2944=VERTEX_POINT('',#9679);
#2945=VERTEX_POINT('',#9682);
#2946=VERTEX_POINT('',#9684);
#2947=VERTEX_POINT('',#9690);
#2948=VERTEX_POINT('',#9694);
#2949=VERTEX_POINT('',#9698);
#2950=VERTEX_POINT('',#9702);
#2951=VERTEX_POINT('',#9704);
#2952=VERTEX_POINT('',#9706);
#2953=VERTEX_POINT('',#9708);
#2954=VERTEX_POINT('',#9710);
#2955=VERTEX_POINT('',#9712);
#2956=VERTEX_POINT('',#9714);
#2957=VERTEX_POINT('',#9716);
#2958=VERTEX_POINT('',#9718);
#2959=VERTEX_POINT('',#9721);
#2960=VERTEX_POINT('',#9724);
#2961=VERTEX_POINT('',#9728);
#2962=VERTEX_POINT('',#9729);
#2963=VERTEX_POINT('',#9756);
#2964=VERTEX_POINT('',#9758);
#2965=VERTEX_POINT('',#9762);
#2966=VERTEX_POINT('',#9765);
#2967=VERTEX_POINT('',#9768);
#2968=VERTEX_POINT('',#9772);
#2969=VERTEX_POINT('',#9774);
#2970=VERTEX_POINT('',#9777);
#2971=VERTEX_POINT('',#9786);
#2972=VERTEX_POINT('',#9787);
#2973=VERTEX_POINT('',#9789);
#2974=VERTEX_POINT('',#9791);
#2975=VERTEX_POINT('',#9795);
#2976=VERTEX_POINT('',#9796);
#2977=VERTEX_POINT('',#9798);
#2978=VERTEX_POINT('',#9800);
#2979=VERTEX_POINT('',#9814);
#2980=VERTEX_POINT('',#9816);
#2981=VERTEX_POINT('',#9820);
#2982=VERTEX_POINT('',#9822);
#2983=VERTEX_POINT('',#9826);
#2984=VERTEX_POINT('',#9828);
#2985=VERTEX_POINT('',#9832);
#2986=VERTEX_POINT('',#9834);
#2987=VERTEX_POINT('',#9838);
#2988=VERTEX_POINT('',#9840);
#2989=VERTEX_POINT('',#9844);
#2990=VERTEX_POINT('',#9847);
#2991=VERTEX_POINT('',#9849);
#2992=VERTEX_POINT('',#9853);
#2993=VERTEX_POINT('',#9856);
#2994=VERTEX_POINT('',#9860);
#2995=VERTEX_POINT('',#9864);
#2996=VERTEX_POINT('',#9865);
#2997=VERTEX_POINT('',#9867);
#2998=VERTEX_POINT('',#9869);
#2999=VERTEX_POINT('',#9873);
#3000=VERTEX_POINT('',#9874);
#3001=VERTEX_POINT('',#9876);
#3002=VERTEX_POINT('',#9878);
#3003=VERTEX_POINT('',#9882);
#3004=VERTEX_POINT('',#9883);
#3005=VERTEX_POINT('',#9885);
#3006=VERTEX_POINT('',#9887);
#3007=VERTEX_POINT('',#9891);
#3008=VERTEX_POINT('',#9892);
#3009=VERTEX_POINT('',#9894);
#3010=VERTEX_POINT('',#9896);
#3011=VERTEX_POINT('',#9900);
#3012=VERTEX_POINT('',#9901);
#3013=VERTEX_POINT('',#9903);
#3014=VERTEX_POINT('',#9905);
#3015=VERTEX_POINT('',#9909);
#3016=VERTEX_POINT('',#9910);
#3017=VERTEX_POINT('',#9912);
#3018=VERTEX_POINT('',#9914);
#3019=VERTEX_POINT('',#9918);
#3020=VERTEX_POINT('',#9919);
#3021=VERTEX_POINT('',#9921);
#3022=VERTEX_POINT('',#9923);
#3023=VERTEX_POINT('',#9927);
#3024=VERTEX_POINT('',#9930);
#3025=VERTEX_POINT('',#9942);
#3026=VERTEX_POINT('',#9944);
#3027=VERTEX_POINT('',#9948);
#3028=VERTEX_POINT('',#9950);
#3029=VERTEX_POINT('',#9954);
#3030=VERTEX_POINT('',#9955);
#3031=VERTEX_POINT('',#9957);
#3032=VERTEX_POINT('',#9964);
#3033=VERTEX_POINT('',#9993);
#3034=VERTEX_POINT('',#9995);
#3035=VERTEX_POINT('',#10031);
#3036=VERTEX_POINT('',#10033);
#3037=VERTEX_POINT('',#10040);
#3038=VERTEX_POINT('',#10069);
#3039=VERTEX_POINT('',#10071);
#3040=VERTEX_POINT('',#10100);
#3041=VERTEX_POINT('',#10109);
#3042=VERTEX_POINT('',#10111);
#3043=VERTEX_POINT('',#10118);
#3044=VERTEX_POINT('',#10147);
#3045=VERTEX_POINT('',#10149);
#3046=VERTEX_POINT('',#10178);
#3047=VERTEX_POINT('',#10187);
#3048=VERTEX_POINT('',#10189);
#3049=VERTEX_POINT('',#10196);
#3050=VERTEX_POINT('',#10225);
#3051=VERTEX_POINT('',#10227);
#3052=VERTEX_POINT('',#10256);
#3053=VERTEX_POINT('',#10265);
#3054=VERTEX_POINT('',#10267);
#3055=VERTEX_POINT('',#10272);
#3056=VERTEX_POINT('',#10274);
#3057=VERTEX_POINT('',#10295);
#3058=VERTEX_POINT('',#10304);
#3059=VERTEX_POINT('',#10310);
#3060=VERTEX_POINT('',#10312);
#3061=VERTEX_POINT('',#10345);
#3062=VERTEX_POINT('',#10347);
#3063=VERTEX_POINT('',#10379);
#3064=VERTEX_POINT('',#10384);
#3065=VERTEX_POINT('',#10416);
#3066=VERTEX_POINT('',#10418);
#3067=VERTEX_POINT('',#10450);
#3068=VERTEX_POINT('',#10455);
#3069=VERTEX_POINT('',#10488);
#3070=VERTEX_POINT('',#10517);
#3071=VERTEX_POINT('',#10523);
#3072=VERTEX_POINT('',#10529);
#3073=VERTEX_POINT('',#10538);
#3074=VERTEX_POINT('',#10539);
#3075=VERTEX_POINT('',#10544);
#3076=VERTEX_POINT('',#10570);
#3077=VERTEX_POINT('',#10572);
#3078=VERTEX_POINT('',#10598);
#3079=VERTEX_POINT('',#10605);
#3080=VERTEX_POINT('',#10609);
#3081=VERTEX_POINT('',#10613);
#3082=VERTEX_POINT('',#10620);
#3083=VERTEX_POINT('',#10627);
#3084=VERTEX_POINT('',#10656);
#3085=VERTEX_POINT('',#10722);
#3086=VERTEX_POINT('',#10775);
#3087=VERTEX_POINT('',#10787);
#3088=VERTEX_POINT('',#10849);
#3089=VERTEX_POINT('',#10859);
#3090=VERTEX_POINT('',#10866);
#3091=VERTEX_POINT('',#10895);
#3092=VERTEX_POINT('',#10897);
#3093=VERTEX_POINT('',#11022);
#3094=VERTEX_POINT('',#11029);
#3095=VERTEX_POINT('',#11058);
#3096=VERTEX_POINT('',#11060);
#3097=VERTEX_POINT('',#11185);
#3098=VERTEX_POINT('',#11192);
#3099=VERTEX_POINT('',#11221);
#3100=VERTEX_POINT('',#11223);
#3101=VERTEX_POINT('',#11274);
#3102=VERTEX_POINT('',#11303);
#3103=VERTEX_POINT('',#11310);
#3104=VERTEX_POINT('',#11332);
#3105=VERTEX_POINT('',#11367);
#3106=VERTEX_POINT('',#11395);
#3107=VERTEX_POINT('',#11490);
#3108=VERTEX_POINT('',#11491);
#3109=VERTEX_POINT('',#11493);
#3110=VERTEX_POINT('',#11497);
#3111=VERTEX_POINT('',#11498);
#3112=VERTEX_POINT('',#11500);
#3113=VERTEX_POINT('',#11504);
#3114=VERTEX_POINT('',#11505);
#3115=VERTEX_POINT('',#11507);
#3116=VERTEX_POINT('',#11542);
#3117=VERTEX_POINT('',#11543);
#3118=VERTEX_POINT('',#11545);
#3119=VERTEX_POINT('',#11749);
#3120=VERTEX_POINT('',#11751);
#3121=VERTEX_POINT('',#11755);
#3122=VERTEX_POINT('',#11757);
#3123=VERTEX_POINT('',#11761);
#3124=VERTEX_POINT('',#11763);
#3125=VERTEX_POINT('',#11767);
#3126=VERTEX_POINT('',#11769);
#3127=VERTEX_POINT('',#11773);
#3128=VERTEX_POINT('',#11774);
#3129=VERTEX_POINT('',#11776);
#3130=VERTEX_POINT('',#11778);
#3131=VERTEX_POINT('',#11782);
#3132=VERTEX_POINT('',#11784);
#3133=VERTEX_POINT('',#11788);
#3134=VERTEX_POINT('',#11790);
#3135=VERTEX_POINT('',#11794);
#3136=VERTEX_POINT('',#11796);
#3137=VERTEX_POINT('',#11800);
#3138=VERTEX_POINT('',#11802);
#3139=VERTEX_POINT('',#11809);
#3140=VERTEX_POINT('',#11812);
#3141=VERTEX_POINT('',#11813);
#3142=VERTEX_POINT('',#11815);
#3143=VERTEX_POINT('',#11817);
#3144=VERTEX_POINT('',#11821);
#3145=VERTEX_POINT('',#11823);
#3146=VERTEX_POINT('',#11827);
#3147=VERTEX_POINT('',#11829);
#3148=VERTEX_POINT('',#11833);
#3149=VERTEX_POINT('',#11835);
#3150=VERTEX_POINT('',#11839);
#3151=VERTEX_POINT('',#11841);
#3152=VERTEX_POINT('',#11848);
#3153=VERTEX_POINT('',#11851);
#3154=VERTEX_POINT('',#11855);
#3155=VERTEX_POINT('',#11859);
#3156=VERTEX_POINT('',#11860);
#3157=VERTEX_POINT('',#11862);
#3158=VERTEX_POINT('',#11864);
#3159=VERTEX_POINT('',#11868);
#3160=VERTEX_POINT('',#11869);
#3161=VERTEX_POINT('',#11871);
#3162=VERTEX_POINT('',#11873);
#3163=VERTEX_POINT('',#11877);
#3164=VERTEX_POINT('',#11878);
#3165=VERTEX_POINT('',#11880);
#3166=VERTEX_POINT('',#11882);
#3167=VERTEX_POINT('',#11886);
#3168=VERTEX_POINT('',#11887);
#3169=VERTEX_POINT('',#11889);
#3170=VERTEX_POINT('',#11891);
#3171=VERTEX_POINT('',#11895);
#3172=VERTEX_POINT('',#11896);
#3173=VERTEX_POINT('',#11898);
#3174=VERTEX_POINT('',#11900);
#3175=VERTEX_POINT('',#11904);
#3176=VERTEX_POINT('',#11905);
#3177=VERTEX_POINT('',#11907);
#3178=VERTEX_POINT('',#11909);
#3179=VERTEX_POINT('',#11913);
#3180=VERTEX_POINT('',#11914);
#3181=VERTEX_POINT('',#11916);
#3182=VERTEX_POINT('',#11918);
#3183=VERTEX_POINT('',#11922);
#3184=VERTEX_POINT('',#11925);
#3185=VERTEX_POINT('',#11937);
#3186=VERTEX_POINT('',#11939);
#3187=VERTEX_POINT('',#11943);
#3188=VERTEX_POINT('',#11945);
#3189=VERTEX_POINT('',#11949);
#3190=VERTEX_POINT('',#11950);
#3191=VERTEX_POINT('',#11952);
#3192=VERTEX_POINT('',#11959);
#3193=VERTEX_POINT('',#11988);
#3194=VERTEX_POINT('',#11990);
#3195=VERTEX_POINT('',#12026);
#3196=VERTEX_POINT('',#12028);
#3197=VERTEX_POINT('',#12035);
#3198=VERTEX_POINT('',#12064);
#3199=VERTEX_POINT('',#12066);
#3200=VERTEX_POINT('',#12095);
#3201=VERTEX_POINT('',#12104);
#3202=VERTEX_POINT('',#12106);
#3203=VERTEX_POINT('',#12113);
#3204=VERTEX_POINT('',#12142);
#3205=VERTEX_POINT('',#12144);
#3206=VERTEX_POINT('',#12173);
#3207=VERTEX_POINT('',#12182);
#3208=VERTEX_POINT('',#12184);
#3209=VERTEX_POINT('',#12191);
#3210=VERTEX_POINT('',#12220);
#3211=VERTEX_POINT('',#12222);
#3212=VERTEX_POINT('',#12251);
#3213=VERTEX_POINT('',#12260);
#3214=VERTEX_POINT('',#12262);
#3215=VERTEX_POINT('',#12267);
#3216=VERTEX_POINT('',#12269);
#3217=VERTEX_POINT('',#12290);
#3218=VERTEX_POINT('',#12299);
#3219=VERTEX_POINT('',#12305);
#3220=VERTEX_POINT('',#12307);
#3221=VERTEX_POINT('',#12340);
#3222=VERTEX_POINT('',#12342);
#3223=VERTEX_POINT('',#12374);
#3224=VERTEX_POINT('',#12379);
#3225=VERTEX_POINT('',#12411);
#3226=VERTEX_POINT('',#12413);
#3227=VERTEX_POINT('',#12445);
#3228=VERTEX_POINT('',#12450);
#3229=VERTEX_POINT('',#12483);
#3230=VERTEX_POINT('',#12512);
#3231=VERTEX_POINT('',#12518);
#3232=VERTEX_POINT('',#12524);
#3233=VERTEX_POINT('',#12533);
#3234=VERTEX_POINT('',#12534);
#3235=VERTEX_POINT('',#12539);
#3236=VERTEX_POINT('',#12565);
#3237=VERTEX_POINT('',#12567);
#3238=VERTEX_POINT('',#12593);
#3239=VERTEX_POINT('',#12600);
#3240=VERTEX_POINT('',#12604);
#3241=VERTEX_POINT('',#12608);
#3242=VERTEX_POINT('',#12615);
#3243=VERTEX_POINT('',#12622);
#3244=VERTEX_POINT('',#12651);
#3245=VERTEX_POINT('',#12717);
#3246=VERTEX_POINT('',#12770);
#3247=VERTEX_POINT('',#12782);
#3248=VERTEX_POINT('',#12844);
#3249=VERTEX_POINT('',#12854);
#3250=VERTEX_POINT('',#12861);
#3251=VERTEX_POINT('',#12890);
#3252=VERTEX_POINT('',#12892);
#3253=VERTEX_POINT('',#13017);
#3254=VERTEX_POINT('',#13024);
#3255=VERTEX_POINT('',#13053);
#3256=VERTEX_POINT('',#13055);
#3257=VERTEX_POINT('',#13180);
#3258=VERTEX_POINT('',#13187);
#3259=VERTEX_POINT('',#13216);
#3260=VERTEX_POINT('',#13218);
#3261=VERTEX_POINT('',#13269);
#3262=VERTEX_POINT('',#13298);
#3263=VERTEX_POINT('',#13305);
#3264=VERTEX_POINT('',#13327);
#3265=VERTEX_POINT('',#13362);
#3266=VERTEX_POINT('',#13390);
#3267=VERTEX_POINT('',#13485);
#3268=VERTEX_POINT('',#13486);
#3269=VERTEX_POINT('',#13488);
#3270=VERTEX_POINT('',#13492);
#3271=VERTEX_POINT('',#13493);
#3272=VERTEX_POINT('',#13495);
#3273=VERTEX_POINT('',#13499);
#3274=VERTEX_POINT('',#13500);
#3275=VERTEX_POINT('',#13502);
#3276=VERTEX_POINT('',#13537);
#3277=VERTEX_POINT('',#13538);
#3278=VERTEX_POINT('',#13540);
#3279=VERTEX_POINT('',#13744);
#3280=VERTEX_POINT('',#13746);
#3281=VERTEX_POINT('',#13750);
#3282=VERTEX_POINT('',#13752);
#3283=VERTEX_POINT('',#13756);
#3284=VERTEX_POINT('',#13758);
#3285=VERTEX_POINT('',#13761);
#3286=VERTEX_POINT('',#13766);
#3287=VERTEX_POINT('',#13768);
#3288=VERTEX_POINT('',#13771);
#3289=VERTEX_POINT('',#13776);
#3290=VERTEX_POINT('',#13778);
#3291=VERTEX_POINT('',#13781);
#3292=VERTEX_POINT('',#13786);
#3293=VERTEX_POINT('',#13788);
#3294=VERTEX_POINT('',#13791);
#3295=VERTEX_POINT('',#13796);
#3296=VERTEX_POINT('',#13800);
#3297=VERTEX_POINT('',#13804);
#3298=VERTEX_POINT('',#13808);
#3299=VERTEX_POINT('',#13836);
#3300=VERTEX_POINT('',#13837);
#3301=VERTEX_POINT('',#13839);
#3302=VERTEX_POINT('',#13845);
#3303=VERTEX_POINT('',#13853);
#3304=VERTEX_POINT('',#13854);
#3305=VERTEX_POINT('',#13883);
#3306=VERTEX_POINT('',#13884);
#3307=VERTEX_POINT('',#13926);
#3308=VERTEX_POINT('',#13927);
#3309=VERTEX_POINT('',#13966);
#3310=VERTEX_POINT('',#13967);
#3311=VERTEX_POINT('',#13980);
#3312=VERTEX_POINT('',#13981);
#3313=VERTEX_POINT('',#14010);
#3314=VERTEX_POINT('',#14011);
#3315=VERTEX_POINT('',#14066);
#3316=VERTEX_POINT('',#14071);
#3317=VERTEX_POINT('',#14097);
#3318=VERTEX_POINT('',#14143);
#3319=VERTEX_POINT('',#14172);
#3320=VERTEX_POINT('',#14207);
#3321=VERTEX_POINT('',#14233);
#3322=VERTEX_POINT('',#14283);
#3323=VERTEX_POINT('',#14339);
#3324=VERTEX_POINT('',#14340);
#3325=VERTEX_POINT('',#14342);
#3326=VERTEX_POINT('',#14353);
#3327=VERTEX_POINT('',#14363);
#3328=VERTEX_POINT('',#14364);
#3329=VERTEX_POINT('',#14411);
#3330=VERTEX_POINT('',#14412);
#3331=VERTEX_POINT('',#14459);
#3332=VERTEX_POINT('',#14460);
#3333=VERTEX_POINT('',#14510);
#3334=VERTEX_POINT('',#14511);
#3335=VERTEX_POINT('',#14558);
#3336=VERTEX_POINT('',#14559);
#3337=VERTEX_POINT('',#14606);
#3338=VERTEX_POINT('',#14607);
#3339=VERTEX_POINT('',#14654);
#3340=VERTEX_POINT('',#14655);
#3341=VERTEX_POINT('',#14708);
#3342=VERTEX_POINT('',#14709);
#3343=VERTEX_POINT('',#14756);
#3344=VERTEX_POINT('',#14757);
#3345=VERTEX_POINT('',#14804);
#3346=VERTEX_POINT('',#14805);
#3347=VERTEX_POINT('',#14858);
#3348=VERTEX_POINT('',#14859);
#3349=VERTEX_POINT('',#14906);
#3350=VERTEX_POINT('',#14907);
#3351=VERTEX_POINT('',#14954);
#3352=VERTEX_POINT('',#14955);
#3353=VERTEX_POINT('',#15002);
#3354=VERTEX_POINT('',#15003);
#3355=VERTEX_POINT('',#15056);
#3356=VERTEX_POINT('',#15057);
#3357=VERTEX_POINT('',#15104);
#3358=VERTEX_POINT('',#15105);
#3359=VERTEX_POINT('',#15152);
#3360=VERTEX_POINT('',#15153);
#3361=VERTEX_POINT('',#15206);
#3362=VERTEX_POINT('',#15207);
#3363=VERTEX_POINT('',#15254);
#3364=VERTEX_POINT('',#15255);
#3365=VERTEX_POINT('',#15302);
#3366=VERTEX_POINT('',#15303);
#3367=VERTEX_POINT('',#15356);
#3368=VERTEX_POINT('',#15357);
#3369=VERTEX_POINT('',#15404);
#3370=VERTEX_POINT('',#15405);
#3371=VERTEX_POINT('',#15452);
#3372=VERTEX_POINT('',#15453);
#3373=VERTEX_POINT('',#15500);
#3374=VERTEX_POINT('',#15501);
#3375=VERTEX_POINT('',#15554);
#3376=VERTEX_POINT('',#15555);
#3377=VERTEX_POINT('',#15602);
#3378=VERTEX_POINT('',#15603);
#3379=VERTEX_POINT('',#15650);
#3380=VERTEX_POINT('',#15651);
#3381=VERTEX_POINT('',#15704);
#3382=VERTEX_POINT('',#15705);
#3383=VERTEX_POINT('',#15752);
#3384=VERTEX_POINT('',#15753);
#3385=VERTEX_POINT('',#15800);
#3386=VERTEX_POINT('',#15801);
#3387=VERTEX_POINT('',#15803);
#3388=VERTEX_POINT('',#15814);
#3389=VERTEX_POINT('',#15826);
#3390=VERTEX_POINT('',#15827);
#3391=VERTEX_POINT('',#15850);
#3392=VERTEX_POINT('',#15851);
#3393=VERTEX_POINT('',#15874);
#3394=VERTEX_POINT('',#15875);
#3395=VERTEX_POINT('',#15899);
#3396=VERTEX_POINT('',#15900);
#3397=VERTEX_POINT('',#15924);
#3398=VERTEX_POINT('',#15925);
#3399=VERTEX_POINT('',#15948);
#3400=VERTEX_POINT('',#15949);
#3401=VERTEX_POINT('',#15973);
#3402=VERTEX_POINT('',#15974);
#3403=VERTEX_POINT('',#15998);
#3404=VERTEX_POINT('',#15999);
#3405=VERTEX_POINT('',#16022);
#3406=VERTEX_POINT('',#16023);
#3407=VERTEX_POINT('',#16046);
#3408=VERTEX_POINT('',#16047);
#3409=VERTEX_POINT('',#16071);
#3410=VERTEX_POINT('',#16072);
#3411=VERTEX_POINT('',#16096);
#3412=VERTEX_POINT('',#16097);
#3413=VERTEX_POINT('',#16120);
#3414=VERTEX_POINT('',#16121);
#3415=VERTEX_POINT('',#16145);
#3416=VERTEX_POINT('',#16146);
#3417=VERTEX_POINT('',#16170);
#3418=VERTEX_POINT('',#16171);
#3419=VERTEX_POINT('',#16194);
#3420=VERTEX_POINT('',#16195);
#3421=VERTEX_POINT('',#16219);
#3422=VERTEX_POINT('',#16220);
#3423=VERTEX_POINT('',#16244);
#3424=VERTEX_POINT('',#16245);
#3425=VERTEX_POINT('',#16268);
#3426=VERTEX_POINT('',#16269);
#3427=VERTEX_POINT('',#16292);
#3428=VERTEX_POINT('',#16293);
#3429=VERTEX_POINT('',#16317);
#3430=VERTEX_POINT('',#16318);
#3431=VERTEX_POINT('',#16342);
#3432=VERTEX_POINT('',#16343);
#3433=VERTEX_POINT('',#16366);
#3434=VERTEX_POINT('',#16367);
#3435=VERTEX_POINT('',#16391);
#3436=VERTEX_POINT('',#16392);
#3437=VERTEX_POINT('',#16416);
#3438=VERTEX_POINT('',#16417);
#3439=VERTEX_POINT('',#16440);
#3440=VERTEX_POINT('',#16441);
#3441=VERTEX_POINT('',#16465);
#3442=VERTEX_POINT('',#16466);
#3443=VERTEX_POINT('',#16489);
#3444=VERTEX_POINT('',#16490);
#3445=VERTEX_POINT('',#16514);
#3446=VERTEX_POINT('',#16515);
#3447=VERTEX_POINT('',#16538);
#3448=VERTEX_POINT('',#16660);
#3449=VERTEX_POINT('',#16698);
#3450=VERTEX_POINT('',#16716);
#3451=VERTEX_POINT('',#17503);
#3452=VERTEX_POINT('',#17581);
#3453=VERTEX_POINT('',#18460);
#3454=VERTEX_POINT('',#18461);
#3455=VERTEX_POINT('',#18463);
#3456=VERTEX_POINT('',#18465);
#3457=VERTEX_POINT('',#18469);
#3458=VERTEX_POINT('',#18471);
#3459=VERTEX_POINT('',#18475);
#3460=VERTEX_POINT('',#18477);
#3461=VERTEX_POINT('',#18481);
#3462=VERTEX_POINT('',#18483);
#3463=VERTEX_POINT('',#18487);
#3464=VERTEX_POINT('',#18489);
#3465=VERTEX_POINT('',#18497);
#3466=VERTEX_POINT('',#18500);
#3467=VERTEX_POINT('',#18507);
#3468=VERTEX_POINT('',#18508);
#3469=VERTEX_POINT('',#18510);
#3470=VERTEX_POINT('',#18520);
#3471=VERTEX_POINT('',#18521);
#3472=VERTEX_POINT('',#18523);
#3473=VERTEX_POINT('',#18567);
#3474=VERTEX_POINT('',#18568);
#3475=VERTEX_POINT('',#18621);
#3476=VERTEX_POINT('',#18622);
#3477=VERTEX_POINT('',#18669);
#3478=VERTEX_POINT('',#18670);
#3479=VERTEX_POINT('',#18672);
#3480=VERTEX_POINT('',#18686);
#3481=VERTEX_POINT('',#18708);
#3482=VERTEX_POINT('',#18709);
#3483=VERTEX_POINT('',#18711);
#3484=VERTEX_POINT('',#18719);
#3485=VERTEX_POINT('',#18729);
#3486=VERTEX_POINT('',#18730);
#3487=VERTEX_POINT('',#18754);
#3488=VERTEX_POINT('',#18755);
#3489=VERTEX_POINT('',#18779);
#3490=VERTEX_POINT('',#18780);
#3491=VERTEX_POINT('',#18804);
#3492=VERTEX_POINT('',#18805);
#3493=VERTEX_POINT('',#18807);
#3494=VERTEX_POINT('',#18813);
#3495=VERTEX_POINT('',#19377);
#3496=VERTEX_POINT('',#19378);
#3497=VERTEX_POINT('',#19380);
#3498=VERTEX_POINT('',#19382);
#3499=VERTEX_POINT('',#19384);
#3500=VERTEX_POINT('',#19386);
#3501=VERTEX_POINT('',#19391);
#3502=VERTEX_POINT('',#19392);
#3503=VERTEX_POINT('',#19397);
#3504=VERTEX_POINT('',#19401);
#3505=VERTEX_POINT('',#19405);
#3506=VERTEX_POINT('',#19409);
#3507=VERTEX_POINT('',#19425);
#3508=VERTEX_POINT('',#19427);
#3509=VERTEX_POINT('',#19431);
#3510=VERTEX_POINT('',#19433);
#3511=EDGE_CURVE('',#2847,#2847,#2657,.T.);
#3512=EDGE_CURVE('',#2847,#2848,#1709,.T.);
#3513=EDGE_CURVE('',#2848,#2848,#2658,.T.);
#3514=EDGE_CURVE('',#2849,#2849,#2659,.T.);
#3515=EDGE_CURVE('',#2849,#2850,#1710,.T.);
#3516=EDGE_CURVE('',#2850,#2850,#2660,.T.);
#3517=EDGE_CURVE('',#2851,#2851,#2661,.T.);
#3518=EDGE_CURVE('',#2851,#2852,#1711,.T.);
#3519=EDGE_CURVE('',#2852,#2852,#2662,.T.);
#3520=EDGE_CURVE('',#2853,#2854,#1712,.T.);
#3521=EDGE_CURVE('',#2855,#2853,#1713,.T.);
#3522=EDGE_CURVE('',#2855,#2854,#1714,.T.);
#3523=EDGE_CURVE('',#2856,#2857,#1715,.T.);
#3524=EDGE_CURVE('',#2855,#2856,#1716,.T.);
#3525=EDGE_CURVE('',#2857,#2853,#1717,.T.);
#3526=EDGE_CURVE('',#2858,#2857,#1718,.T.);
#3527=EDGE_CURVE('',#2856,#2858,#1719,.T.);
#3528=EDGE_CURVE('',#2854,#2859,#1720,.T.);
#3529=EDGE_CURVE('',#2859,#2860,#1721,.T.);
#3530=EDGE_CURVE('',#2860,#2861,#1722,.T.);
#3531=EDGE_CURVE('',#2861,#2862,#1723,.T.);
#3532=EDGE_CURVE('',#2862,#2863,#1724,.T.);
#3533=EDGE_CURVE('',#2863,#2857,#2663,.T.);
#3534=EDGE_CURVE('',#2859,#2864,#1725,.T.);
#3535=EDGE_CURVE('',#2864,#2855,#1726,.T.);
#3536=EDGE_CURVE('',#2865,#2856,#2664,.T.);
#3537=EDGE_CURVE('',#2857,#2858,#2665,.T.);
#3538=EDGE_CURVE('',#2865,#2857,#1727,.T.);
#3539=EDGE_CURVE('',#2866,#2865,#2666,.T.);
#3540=EDGE_CURVE('',#2866,#2863,#1728,.T.);
#3541=EDGE_CURVE('',#2864,#2867,#1729,.T.);
#3542=EDGE_CURVE('',#2866,#2867,#1730,.T.);
#3543=EDGE_CURVE('',#2868,#2867,#1731,.T.);
#3544=EDGE_CURVE('',#2869,#2868,#1732,.T.);
#3545=EDGE_CURVE('',#2869,#2860,#1733,.T.);
#3546=EDGE_CURVE('',#2870,#2862,#1734,.T.);
#3547=EDGE_CURVE('',#2871,#2870,#1735,.T.);
#3548=EDGE_CURVE('',#2872,#2871,#1736,.T.);
#3549=EDGE_CURVE('',#2868,#2872,#1737,.T.);
#3550=EDGE_CURVE('',#2873,#2861,#1738,.T.);
#3551=EDGE_CURVE('',#2870,#2873,#1739,.T.);
#3552=EDGE_CURVE('',#2874,#2869,#1740,.T.);
#3553=EDGE_CURVE('',#2875,#2874,#1741,.T.);
#3554=EDGE_CURVE('',#2873,#2875,#1742,.T.);
#3555=EDGE_CURVE('',#2872,#2876,#1743,.T.);
#3556=EDGE_CURVE('',#2877,#2876,#2667,.T.);
#3557=EDGE_CURVE('',#2878,#2877,#1744,.T.);
#3558=EDGE_CURVE('',#2879,#2878,#1745,.T.);
#3559=EDGE_CURVE('',#2880,#2879,#2668,.T.);
#3560=EDGE_CURVE('',#2881,#2880,#1746,.T.);
#3561=EDGE_CURVE('',#2882,#2881,#1747,.T.);
#3562=EDGE_CURVE('',#2883,#2882,#1748,.T.);
#3563=EDGE_CURVE('',#2884,#2883,#1749,.T.);
#3564=EDGE_CURVE('',#2885,#2884,#1750,.T.);
#3565=EDGE_CURVE('',#2886,#2885,#2669,.T.);
#3566=EDGE_CURVE('',#2887,#2886,#1751,.T.);
#3567=EDGE_CURVE('',#2874,#2887,#2670,.T.);
#3568=EDGE_CURVE('',#2888,#2888,#2671,.T.);
#3569=EDGE_CURVE('',#2876,#2889,#1752,.T.);
#3570=EDGE_CURVE('',#2889,#2871,#1753,.T.);
#3571=EDGE_CURVE('',#2887,#2890,#1754,.T.);
#3572=EDGE_CURVE('',#2875,#2890,#2672,.T.);
#3573=EDGE_CURVE('',#2891,#2889,#2673,.T.);
#3574=EDGE_CURVE('',#2891,#2877,#1755,.T.);
#3575=EDGE_CURVE('',#2890,#2892,#1756,.T.);
#3576=EDGE_CURVE('',#2892,#2893,#2674,.T.);
#3577=EDGE_CURVE('',#2893,#2894,#1757,.T.);
#3578=EDGE_CURVE('',#2894,#2895,#1758,.T.);
#3579=EDGE_CURVE('',#2895,#2896,#1759,.T.);
#3580=EDGE_CURVE('',#2896,#2897,#1760,.T.);
#3581=EDGE_CURVE('',#2897,#2898,#1761,.T.);
#3582=EDGE_CURVE('',#2898,#2899,#2675,.T.);
#3583=EDGE_CURVE('',#2899,#2900,#1762,.T.);
#3584=EDGE_CURVE('',#2900,#2891,#1763,.T.);
#3585=EDGE_CURVE('',#2901,#2901,#2676,.T.);
#3586=EDGE_CURVE('',#2888,#2902,#2677,.T.);
#3587=EDGE_CURVE('',#2902,#2902,#2678,.T.);
#3588=EDGE_CURVE('',#2903,#2904,#2679,.T.);
#3589=EDGE_CURVE('',#2904,#2903,#2680,.T.);
#3590=EDGE_CURVE('',#2904,#2902,#1764,.T.);
#3591=EDGE_CURVE('',#2901,#2903,#2681,.T.);
#3592=EDGE_CURVE('',#2899,#2879,#1765,.T.);
#3593=EDGE_CURVE('',#2880,#2898,#1766,.T.);
#3594=EDGE_CURVE('',#2886,#2892,#1767,.T.);
#3595=EDGE_CURVE('',#2893,#2885,#1768,.T.);
#3596=EDGE_CURVE('',#2884,#2894,#1769,.T.);
#3597=EDGE_CURVE('',#2881,#2897,#1770,.T.);
#3598=EDGE_CURVE('',#2878,#2900,#1771,.T.);
#3599=EDGE_CURVE('',#2882,#2896,#1772,.T.);
#3600=EDGE_CURVE('',#2883,#2895,#1773,.T.);
#3601=EDGE_CURVE('',#2905,#2905,#2682,.T.);
#3602=EDGE_CURVE('',#2905,#2906,#1774,.T.);
#3603=EDGE_CURVE('',#2906,#2906,#2683,.T.);
#3604=EDGE_CURVE('',#2907,#2907,#2684,.T.);
#3605=EDGE_CURVE('',#2907,#2908,#1775,.T.);
#3606=EDGE_CURVE('',#2908,#2908,#2685,.T.);
#3607=EDGE_CURVE('',#2909,#2909,#2686,.T.);
#3608=EDGE_CURVE('',#2909,#2910,#1776,.T.);
#3609=EDGE_CURVE('',#2910,#2910,#2687,.T.);
#3610=EDGE_CURVE('',#2911,#2912,#1777,.T.);
#3611=EDGE_CURVE('',#2913,#2911,#1778,.T.);
#3612=EDGE_CURVE('',#2913,#2912,#1779,.T.);
#3613=EDGE_CURVE('',#2914,#2915,#1780,.T.);
#3614=EDGE_CURVE('',#2913,#2914,#1781,.T.);
#3615=EDGE_CURVE('',#2915,#2911,#1782,.T.);
#3616=EDGE_CURVE('',#2916,#2915,#1783,.T.);
#3617=EDGE_CURVE('',#2914,#2916,#1784,.T.);
#3618=EDGE_CURVE('',#2912,#2917,#1785,.T.);
#3619=EDGE_CURVE('',#2918,#2917,#1786,.T.);
#3620=EDGE_CURVE('',#2918,#2919,#1787,.T.);
#3621=EDGE_CURVE('',#2919,#2915,#2688,.T.);
#3622=EDGE_CURVE('',#2915,#2916,#2689,.T.);
#3623=EDGE_CURVE('',#2917,#2920,#1788,.T.);
#3624=EDGE_CURVE('',#2920,#2913,#1789,.T.);
#3625=EDGE_CURVE('',#2921,#2914,#2690,.T.);
#3626=EDGE_CURVE('',#2921,#2915,#1790,.T.);
#3627=EDGE_CURVE('',#2922,#2921,#2691,.T.);
#3628=EDGE_CURVE('',#2922,#2919,#1791,.T.);
#3629=EDGE_CURVE('',#2923,#2924,#1792,.T.);
#3630=EDGE_CURVE('',#2924,#2925,#1793,.T.);
#3631=EDGE_CURVE('',#2925,#2920,#1794,.T.);
#3632=EDGE_CURVE('',#2922,#2923,#1795,.T.);
#3633=EDGE_CURVE('',#2923,#2926,#1796,.T.);
#3634=EDGE_CURVE('',#2927,#2926,#1797,.T.);
#3635=EDGE_CURVE('',#2924,#2927,#1798,.T.);
#3636=EDGE_CURVE('',#2928,#2927,#1799,.T.);
#3637=EDGE_CURVE('',#2929,#2928,#1800,.T.);
#3638=EDGE_CURVE('',#2930,#2929,#1801,.T.);
#3639=EDGE_CURVE('',#2925,#2930,#1802,.T.);
#3640=EDGE_CURVE('',#2926,#2931,#1803,.T.);
#3641=EDGE_CURVE('',#2931,#2932,#1804,.T.);
#3642=EDGE_CURVE('',#2933,#2932,#2692,.T.);
#3643=EDGE_CURVE('',#2934,#2933,#1805,.T.);
#3644=EDGE_CURVE('',#2935,#2934,#1806,.T.);
#3645=EDGE_CURVE('',#2936,#2935,#2693,.T.);
#3646=EDGE_CURVE('',#2937,#2936,#1807,.T.);
#3647=EDGE_CURVE('',#2938,#2937,#1808,.T.);
#3648=EDGE_CURVE('',#2939,#2938,#1809,.T.);
#3649=EDGE_CURVE('',#2940,#2939,#1810,.T.);
#3650=EDGE_CURVE('',#2941,#2940,#1811,.T.);
#3651=EDGE_CURVE('',#2942,#2941,#2694,.T.);
#3652=EDGE_CURVE('',#2943,#2942,#1812,.T.);
#3653=EDGE_CURVE('',#2928,#2943,#2695,.T.);
#3654=EDGE_CURVE('',#2944,#2944,#2696,.T.);
#3655=EDGE_CURVE('',#2918,#2945,#1813,.T.);
#3656=EDGE_CURVE('',#2946,#2945,#1814,.T.);
#3657=EDGE_CURVE('',#2931,#2946,#1815,.T.);
#3658=EDGE_CURVE('',#2945,#2930,#1816,.T.);
#3659=EDGE_CURVE('',#2932,#2947,#1817,.T.);
#3660=EDGE_CURVE('',#2947,#2946,#1818,.T.);
#3661=EDGE_CURVE('',#2943,#2948,#1819,.T.);
#3662=EDGE_CURVE('',#2929,#2948,#2697,.T.);
#3663=EDGE_CURVE('',#2949,#2947,#2698,.T.);
#3664=EDGE_CURVE('',#2949,#2933,#1820,.T.);
#3665=EDGE_CURVE('',#2948,#2950,#1821,.T.);
#3666=EDGE_CURVE('',#2950,#2951,#2699,.T.);
#3667=EDGE_CURVE('',#2951,#2952,#1822,.T.);
#3668=EDGE_CURVE('',#2952,#2953,#1823,.T.);
#3669=EDGE_CURVE('',#2953,#2954,#1824,.T.);
#3670=EDGE_CURVE('',#2954,#2955,#1825,.T.);
#3671=EDGE_CURVE('',#2955,#2956,#1826,.T.);
#3672=EDGE_CURVE('',#2956,#2957,#2700,.T.);
#3673=EDGE_CURVE('',#2957,#2958,#1827,.T.);
#3674=EDGE_CURVE('',#2958,#2949,#1828,.T.);
#3675=EDGE_CURVE('',#2959,#2959,#2701,.T.);
#3676=EDGE_CURVE('',#2944,#2960,#2702,.T.);
#3677=EDGE_CURVE('',#2960,#2960,#2703,.T.);
#3678=EDGE_CURVE('',#2961,#2962,#2704,.T.);
#3679=EDGE_CURVE('',#2962,#2961,#2705,.T.);
#3680=EDGE_CURVE('',#2962,#2960,#1829,.T.);
#3681=EDGE_CURVE('',#2959,#2961,#2706,.T.);
#3682=EDGE_CURVE('',#2957,#2935,#1830,.T.);
#3683=EDGE_CURVE('',#2936,#2956,#1831,.T.);
#3684=EDGE_CURVE('',#2942,#2950,#1832,.T.);
#3685=EDGE_CURVE('',#2951,#2941,#1833,.T.);
#3686=EDGE_CURVE('',#2940,#2952,#1834,.T.);
#3687=EDGE_CURVE('',#2937,#2955,#1835,.T.);
#3688=EDGE_CURVE('',#2934,#2958,#1836,.T.);
#3689=EDGE_CURVE('',#2938,#2954,#1837,.T.);
#3690=EDGE_CURVE('',#2939,#2953,#1838,.T.);
#3691=EDGE_CURVE('',#2963,#2963,#2707,.T.);
#3692=EDGE_CURVE('',#2963,#2964,#1839,.T.);
#3693=EDGE_CURVE('',#2964,#2964,#2708,.T.);
#3694=EDGE_CURVE('',#2965,#2965,#2709,.T.);
#3695=EDGE_CURVE('',#2966,#2966,#2710,.T.);
#3696=EDGE_CURVE('',#2967,#2967,#2711,.T.);
#3697=EDGE_CURVE('',#2967,#2966,#1840,.T.);
#3698=EDGE_CURVE('',#2968,#2968,#2712,.T.);
#3699=EDGE_CURVE('',#2969,#2969,#2713,.T.);
#3700=EDGE_CURVE('',#2968,#2970,#1841,.T.);
#3701=EDGE_CURVE('',#2970,#2970,#2714,.T.);
#3702=EDGE_CURVE('',#2965,#2969,#1842,.T.);
#3703=EDGE_CURVE('',#2971,#2972,#1843,.T.);
#3704=EDGE_CURVE('',#2973,#2971,#1844,.T.);
#3705=EDGE_CURVE('',#2974,#2973,#1845,.T.);
#3706=EDGE_CURVE('',#2972,#2974,#1846,.T.);
#3707=EDGE_CURVE('',#2975,#2976,#1847,.T.);
#3708=EDGE_CURVE('',#2977,#2975,#1848,.T.);
#3709=EDGE_CURVE('',#2978,#2977,#1849,.T.);
#3710=EDGE_CURVE('',#2976,#2978,#1850,.T.);
#3711=EDGE_CURVE('',#2973,#2978,#2715,.T.);
#3712=EDGE_CURVE('',#2976,#2971,#2716,.T.);
#3713=EDGE_CURVE('',#2975,#2972,#2717,.T.);
#3714=EDGE_CURVE('',#2974,#2977,#2718,.T.);
#3715=EDGE_CURVE('',#2979,#2979,#2719,.T.);
#3716=EDGE_CURVE('',#2979,#2980,#1851,.T.);
#3717=EDGE_CURVE('',#2980,#2980,#2720,.T.);
#3718=EDGE_CURVE('',#2981,#2981,#2721,.T.);
#3719=EDGE_CURVE('',#2981,#2982,#1852,.T.);
#3720=EDGE_CURVE('',#2982,#2982,#2722,.T.);
#3721=EDGE_CURVE('',#2983,#2983,#2723,.T.);
#3722=EDGE_CURVE('',#2983,#2984,#1853,.T.);
#3723=EDGE_CURVE('',#2984,#2984,#2724,.T.);
#3724=EDGE_CURVE('',#2985,#2985,#2725,.T.);
#3725=EDGE_CURVE('',#2985,#2986,#1854,.T.);
#3726=EDGE_CURVE('',#2986,#2986,#2726,.T.);
#3727=EDGE_CURVE('',#2987,#2987,#2727,.T.);
#3728=EDGE_CURVE('',#2987,#2988,#1855,.T.);
#3729=EDGE_CURVE('',#2988,#2988,#2728,.T.);
#3730=EDGE_CURVE('',#2989,#2989,#2729,.T.);
#3731=EDGE_CURVE('',#2990,#2990,#2730,.T.);
#3732=EDGE_CURVE('',#2990,#2991,#1856,.T.);
#3733=EDGE_CURVE('',#2991,#2991,#2731,.T.);
#3734=EDGE_CURVE('',#2992,#2992,#2732,.T.);
#3735=EDGE_CURVE('',#2989,#2993,#1857,.T.);
#3736=EDGE_CURVE('',#2993,#2993,#2733,.T.);
#3737=EDGE_CURVE('',#2992,#2994,#1858,.T.);
#3738=EDGE_CURVE('',#2994,#2994,#2734,.T.);
#3739=EDGE_CURVE('',#2995,#2996,#1859,.T.);
#3740=EDGE_CURVE('',#2997,#2995,#1860,.T.);
#3741=EDGE_CURVE('',#2998,#2997,#1861,.T.);
#3742=EDGE_CURVE('',#2998,#2996,#1862,.T.);
#3743=EDGE_CURVE('',#2999,#3000,#1863,.T.);
#3744=EDGE_CURVE('',#2999,#3001,#1864,.T.);
#3745=EDGE_CURVE('',#3002,#3001,#1865,.T.);
#3746=EDGE_CURVE('',#3000,#3002,#1866,.T.);
#3747=EDGE_CURVE('',#3003,#3004,#1867,.T.);
#3748=EDGE_CURVE('',#3003,#3005,#1868,.T.);
#3749=EDGE_CURVE('',#3006,#3005,#1869,.T.);
#3750=EDGE_CURVE('',#3004,#3006,#1870,.T.);
#3751=EDGE_CURVE('',#3007,#3008,#1871,.T.);
#3752=EDGE_CURVE('',#3007,#3009,#1872,.T.);
#3753=EDGE_CURVE('',#3010,#3009,#1873,.T.);
#3754=EDGE_CURVE('',#3008,#3010,#1874,.T.);
#3755=EDGE_CURVE('',#3011,#3012,#1875,.T.);
#3756=EDGE_CURVE('',#3011,#3013,#1876,.T.);
#3757=EDGE_CURVE('',#3014,#3013,#1877,.T.);
#3758=EDGE_CURVE('',#3012,#3014,#1878,.T.);
#3759=EDGE_CURVE('',#3015,#3016,#1879,.T.);
#3760=EDGE_CURVE('',#3017,#3015,#1880,.T.);
#3761=EDGE_CURVE('',#3018,#3017,#1881,.T.);
#3762=EDGE_CURVE('',#3018,#3016,#1882,.T.);
#3763=EDGE_CURVE('',#3019,#3020,#1883,.T.);
#3764=EDGE_CURVE('',#3021,#3019,#1884,.T.);
#3765=EDGE_CURVE('',#3022,#3021,#1885,.T.);
#3766=EDGE_CURVE('',#3022,#3020,#1886,.T.);
#3767=EDGE_CURVE('',#3023,#3023,#2735,.T.);
#3768=EDGE_CURVE('',#3024,#3024,#2736,.T.);
#3769=EDGE_CURVE('',#2996,#3011,#1887,.T.);
#3770=EDGE_CURVE('',#3013,#2998,#1888,.T.);
#3771=EDGE_CURVE('',#3016,#2999,#1889,.T.);
#3772=EDGE_CURVE('',#3001,#3018,#1890,.T.);
#3773=EDGE_CURVE('',#3020,#3003,#1891,.T.);
#3774=EDGE_CURVE('',#3005,#3022,#1892,.T.);
#3775=EDGE_CURVE('',#3025,#3007,#1893,.T.);
#3776=EDGE_CURVE('',#3026,#3025,#1894,.T.);
#3777=EDGE_CURVE('',#3009,#3026,#1895,.T.);
#3778=EDGE_CURVE('',#3027,#3025,#1896,.T.);
#3779=EDGE_CURVE('',#3028,#3027,#1897,.T.);
#3780=EDGE_CURVE('',#3026,#3028,#1898,.T.);
#3781=EDGE_CURVE('',#3029,#3030,#1899,.T.);
#3782=EDGE_CURVE('',#3031,#3030,#172,.T.);
#3783=EDGE_CURVE('',#3032,#3031,#173,.T.);
#3784=EDGE_CURVE('',#3033,#3032,#1900,.T.);
#3785=EDGE_CURVE('',#3034,#3033,#174,.T.);
#3786=EDGE_CURVE('',#3029,#3034,#175,.T.);
#3787=EDGE_CURVE('',#3028,#3035,#1901,.T.);
#3788=EDGE_CURVE('',#3036,#3035,#176,.T.);
#3789=EDGE_CURVE('',#3037,#3036,#177,.T.);
#3790=EDGE_CURVE('',#3038,#3037,#1902,.T.);
#3791=EDGE_CURVE('',#3039,#3038,#178,.T.);
#3792=EDGE_CURVE('',#3040,#3039,#179,.T.);
#3793=EDGE_CURVE('',#3040,#3010,#1903,.T.);
#3794=EDGE_CURVE('',#3021,#3041,#1904,.T.);
#3795=EDGE_CURVE('',#3042,#3041,#180,.T.);
#3796=EDGE_CURVE('',#3043,#3042,#181,.T.);
#3797=EDGE_CURVE('',#3044,#3043,#1905,.T.);
#3798=EDGE_CURVE('',#3045,#3044,#182,.T.);
#3799=EDGE_CURVE('',#3046,#3045,#183,.T.);
#3800=EDGE_CURVE('',#3046,#3006,#1906,.T.);
#3801=EDGE_CURVE('',#3017,#3047,#1907,.T.);
#3802=EDGE_CURVE('',#3048,#3047,#184,.T.);
#3803=EDGE_CURVE('',#3049,#3048,#185,.T.);
#3804=EDGE_CURVE('',#3050,#3049,#1908,.T.);
#3805=EDGE_CURVE('',#3051,#3050,#186,.T.);
#3806=EDGE_CURVE('',#3052,#3051,#187,.T.);
#3807=EDGE_CURVE('',#3052,#3002,#1909,.T.);
#3808=EDGE_CURVE('',#3053,#3012,#1910,.T.);
#3809=EDGE_CURVE('',#3053,#3054,#188,.T.);
#3810=EDGE_CURVE('',#3054,#3055,#1911,.T.);
#3811=EDGE_CURVE('',#3055,#3056,#189,.T.);
#3812=EDGE_CURVE('',#2995,#3056,#1912,.T.);
#3813=EDGE_CURVE('',#3040,#3030,#190,.T.);
#3814=EDGE_CURVE('',#3029,#3035,#191,.T.);
#3815=EDGE_CURVE('',#3057,#3027,#1913,.T.);
#3816=EDGE_CURVE('',#3057,#3041,#192,.T.);
#3817=EDGE_CURVE('',#3058,#3019,#1914,.T.);
#3818=EDGE_CURVE('',#3058,#3047,#193,.T.);
#3819=EDGE_CURVE('',#3059,#3015,#1915,.T.);
#3820=EDGE_CURVE('',#3059,#3060,#194,.T.);
#3821=EDGE_CURVE('',#3060,#3053,#195,.T.);
#3822=EDGE_CURVE('',#3014,#3061,#1916,.T.);
#3823=EDGE_CURVE('',#3062,#3061,#196,.T.);
#3824=EDGE_CURVE('',#3062,#3063,#197,.T.);
#3825=EDGE_CURVE('',#3064,#3063,#198,.T.);
#3826=EDGE_CURVE('',#3064,#3065,#1917,.T.);
#3827=EDGE_CURVE('',#3066,#3065,#199,.T.);
#3828=EDGE_CURVE('',#3066,#3067,#200,.T.);
#3829=EDGE_CURVE('',#3068,#3067,#201,.T.);
#3830=EDGE_CURVE('',#3068,#2997,#1918,.T.);
#3831=EDGE_CURVE('',#3056,#3069,#202,.T.);
#3832=EDGE_CURVE('',#3069,#3070,#203,.T.);
#3833=EDGE_CURVE('',#3000,#3070,#1919,.T.);
#3834=EDGE_CURVE('',#3052,#3071,#204,.T.);
#3835=EDGE_CURVE('',#3004,#3071,#1920,.T.);
#3836=EDGE_CURVE('',#3046,#3072,#205,.T.);
#3837=EDGE_CURVE('',#3008,#3072,#1921,.T.);
#3838=EDGE_CURVE('',#3073,#3074,#206,.T.);
#3839=EDGE_CURVE('',#3074,#3075,#207,.T.);
#3840=EDGE_CURVE('',#3075,#3076,#1922,.T.);
#3841=EDGE_CURVE('',#3076,#3077,#208,.T.);
#3842=EDGE_CURVE('',#3077,#3078,#209,.T.);
#3843=EDGE_CURVE('',#3073,#3078,#1923,.T.);
#3844=EDGE_CURVE('',#3079,#3079,#2737,.T.);
#3845=EDGE_CURVE('',#3079,#3024,#1924,.T.);
#3846=EDGE_CURVE('',#3080,#3080,#2738,.T.);
#3847=EDGE_CURVE('',#3080,#3023,#1925,.T.);
#3848=EDGE_CURVE('',#3073,#3081,#210,.T.);
#3849=EDGE_CURVE('',#3082,#3078,#211,.T.);
#3850=EDGE_CURVE('',#3083,#3082,#212,.T.);
#3851=EDGE_CURVE('',#3084,#3083,#1926,.T.);
#3852=EDGE_CURVE('',#3081,#3084,#213,.T.);
#3853=EDGE_CURVE('',#3039,#3031,#214,.T.);
#3854=EDGE_CURVE('',#3081,#3085,#215,.T.);
#3855=EDGE_CURVE('',#3085,#3074,#216,.T.);
#3856=EDGE_CURVE('',#3032,#3038,#217,.T.);
#3857=EDGE_CURVE('',#3086,#3084,#218,.T.);
#3858=EDGE_CURVE('',#3085,#3086,#2739,.F.);
#3859=EDGE_CURVE('',#3037,#3033,#219,.T.);
#3860=EDGE_CURVE('',#3083,#3087,#220,.T.);
#3861=EDGE_CURVE('',#3087,#3086,#1927,.T.);
#3862=EDGE_CURVE('',#3034,#3036,#221,.T.);
#3863=EDGE_CURVE('',#3077,#3088,#222,.T.);
#3864=EDGE_CURVE('',#3088,#3082,#223,.T.);
#3865=EDGE_CURVE('',#3089,#3072,#224,.T.);
#3866=EDGE_CURVE('',#3090,#3089,#225,.T.);
#3867=EDGE_CURVE('',#3091,#3090,#1928,.T.);
#3868=EDGE_CURVE('',#3092,#3091,#226,.T.);
#3869=EDGE_CURVE('',#3057,#3092,#227,.T.);
#3870=EDGE_CURVE('',#3045,#3089,#228,.T.);
#3871=EDGE_CURVE('',#3090,#3044,#229,.T.);
#3872=EDGE_CURVE('',#3043,#3091,#230,.T.);
#3873=EDGE_CURVE('',#3092,#3042,#231,.T.);
#3874=EDGE_CURVE('',#3093,#3071,#232,.T.);
#3875=EDGE_CURVE('',#3094,#3093,#233,.T.);
#3876=EDGE_CURVE('',#3095,#3094,#1929,.T.);
#3877=EDGE_CURVE('',#3096,#3095,#234,.T.);
#3878=EDGE_CURVE('',#3058,#3096,#235,.T.);
#3879=EDGE_CURVE('',#3051,#3093,#236,.T.);
#3880=EDGE_CURVE('',#3094,#3050,#237,.T.);
#3881=EDGE_CURVE('',#3049,#3095,#238,.T.);
#3882=EDGE_CURVE('',#3096,#3048,#239,.T.);
#3883=EDGE_CURVE('',#3097,#3070,#240,.T.);
#3884=EDGE_CURVE('',#3098,#3097,#241,.T.);
#3885=EDGE_CURVE('',#3099,#3098,#1930,.T.);
#3886=EDGE_CURVE('',#3100,#3099,#242,.T.);
#3887=EDGE_CURVE('',#3059,#3100,#243,.T.);
#3888=EDGE_CURVE('',#3069,#3101,#244,.T.);
#3889=EDGE_CURVE('',#3101,#3097,#245,.T.);
#3890=EDGE_CURVE('',#3102,#3101,#2740,.F.);
#3891=EDGE_CURVE('',#3098,#3102,#246,.T.);
#3892=EDGE_CURVE('',#3102,#3103,#1931,.T.);
#3893=EDGE_CURVE('',#3103,#3099,#247,.T.);
#3894=EDGE_CURVE('',#3100,#3104,#248,.T.);
#3895=EDGE_CURVE('',#3104,#3060,#249,.T.);
#3896=EDGE_CURVE('',#3104,#3103,#2741,.F.);
#3897=EDGE_CURVE('',#3103,#3054,#2742,.F.);
#3898=EDGE_CURVE('',#3054,#3104,#2743,.F.);
#3899=EDGE_CURVE('',#3087,#3088,#2744,.F.);
#3900=EDGE_CURVE('',#3088,#3105,#2745,.F.);
#3901=EDGE_CURVE('',#3105,#3087,#2746,.F.);
#3902=EDGE_CURVE('',#3101,#3055,#2747,.F.);
#3903=EDGE_CURVE('',#3055,#3102,#2748,.F.);
#3904=EDGE_CURVE('',#3106,#3085,#2749,.F.);
#3905=EDGE_CURVE('',#3086,#3106,#2750,.F.);
#3906=EDGE_CURVE('',#3106,#3105,#1932,.T.);
#3907=EDGE_CURVE('',#3075,#3106,#250,.T.);
#3908=EDGE_CURVE('',#3105,#3076,#251,.T.);
#3909=EDGE_CURVE('',#3107,#3108,#2751,.F.);
#3910=EDGE_CURVE('',#3109,#3107,#2752,.F.);
#3911=EDGE_CURVE('',#3108,#3109,#2753,.F.);
#3912=EDGE_CURVE('',#3110,#3111,#2754,.F.);
#3913=EDGE_CURVE('',#3112,#3110,#2755,.F.);
#3914=EDGE_CURVE('',#3111,#3112,#2756,.F.);
#3915=EDGE_CURVE('',#3113,#3114,#2757,.F.);
#3916=EDGE_CURVE('',#3115,#3113,#2758,.F.);
#3917=EDGE_CURVE('',#3114,#3115,#2759,.F.);
#3918=EDGE_CURVE('',#3108,#3115,#1933,.T.);
#3919=EDGE_CURVE('',#3113,#3107,#1934,.T.);
#3920=EDGE_CURVE('',#3067,#3114,#252,.T.);
#3921=EDGE_CURVE('',#3115,#3068,#253,.T.);
#3922=EDGE_CURVE('',#3116,#3117,#2760,.F.);
#3923=EDGE_CURVE('',#3118,#3116,#2761,.F.);
#3924=EDGE_CURVE('',#3117,#3118,#2762,.F.);
#3925=EDGE_CURVE('',#3116,#3112,#1935,.T.);
#3926=EDGE_CURVE('',#3110,#3118,#1936,.T.);
#3927=EDGE_CURVE('',#3114,#3117,#254,.T.);
#3928=EDGE_CURVE('',#3118,#3113,#255,.T.);
#3929=EDGE_CURVE('',#3065,#3116,#256,.T.);
#3930=EDGE_CURVE('',#3117,#3066,#257,.T.);
#3931=EDGE_CURVE('',#3063,#3111,#258,.T.);
#3932=EDGE_CURVE('',#3112,#3064,#259,.T.);
#3933=EDGE_CURVE('',#3111,#3109,#260,.T.);
#3934=EDGE_CURVE('',#3107,#3110,#261,.T.);
#3935=EDGE_CURVE('',#3061,#3108,#262,.T.);
#3936=EDGE_CURVE('',#3109,#3062,#263,.T.);
#3937=EDGE_CURVE('',#3119,#3119,#2763,.T.);
#3938=EDGE_CURVE('',#3119,#3120,#1937,.T.);
#3939=EDGE_CURVE('',#3120,#3120,#2764,.T.);
#3940=EDGE_CURVE('',#3121,#3121,#2765,.T.);
#3941=EDGE_CURVE('',#3121,#3122,#1938,.T.);
#3942=EDGE_CURVE('',#3122,#3122,#2766,.T.);
#3943=EDGE_CURVE('',#3123,#3123,#2767,.T.);
#3944=EDGE_CURVE('',#3123,#3124,#1939,.T.);
#3945=EDGE_CURVE('',#3124,#3124,#2768,.T.);
#3946=EDGE_CURVE('',#3125,#3125,#2769,.T.);
#3947=EDGE_CURVE('',#3125,#3126,#1940,.T.);
#3948=EDGE_CURVE('',#3126,#3126,#2770,.T.);
#3949=EDGE_CURVE('',#3127,#3128,#1941,.T.);
#3950=EDGE_CURVE('',#3127,#3129,#1942,.T.);
#3951=EDGE_CURVE('',#3129,#3130,#1943,.T.);
#3952=EDGE_CURVE('',#3128,#3130,#1944,.T.);
#3953=EDGE_CURVE('',#3131,#3127,#1945,.T.);
#3954=EDGE_CURVE('',#3131,#3132,#1946,.T.);
#3955=EDGE_CURVE('',#3132,#3129,#1947,.T.);
#3956=EDGE_CURVE('',#3133,#3131,#1948,.T.);
#3957=EDGE_CURVE('',#3133,#3134,#1949,.T.);
#3958=EDGE_CURVE('',#3134,#3132,#1950,.T.);
#3959=EDGE_CURVE('',#3135,#3133,#1951,.T.);
#3960=EDGE_CURVE('',#3135,#3136,#1952,.T.);
#3961=EDGE_CURVE('',#3136,#3134,#1953,.T.);
#3962=EDGE_CURVE('',#3137,#3135,#1954,.T.);
#3963=EDGE_CURVE('',#3137,#3138,#1955,.T.);
#3964=EDGE_CURVE('',#3138,#3136,#1956,.T.);
#3965=EDGE_CURVE('',#3128,#3137,#1957,.T.);
#3966=EDGE_CURVE('',#3130,#3138,#1958,.T.);
#3967=EDGE_CURVE('',#3139,#3139,#2771,.T.);
#3968=EDGE_CURVE('',#3140,#3141,#1959,.T.);
#3969=EDGE_CURVE('',#3140,#3142,#1960,.T.);
#3970=EDGE_CURVE('',#3142,#3143,#1961,.T.);
#3971=EDGE_CURVE('',#3141,#3143,#1962,.T.);
#3972=EDGE_CURVE('',#3144,#3140,#1963,.T.);
#3973=EDGE_CURVE('',#3144,#3145,#1964,.T.);
#3974=EDGE_CURVE('',#3145,#3142,#1965,.T.);
#3975=EDGE_CURVE('',#3146,#3144,#1966,.T.);
#3976=EDGE_CURVE('',#3146,#3147,#1967,.T.);
#3977=EDGE_CURVE('',#3147,#3145,#1968,.T.);
#3978=EDGE_CURVE('',#3148,#3146,#1969,.T.);
#3979=EDGE_CURVE('',#3148,#3149,#1970,.T.);
#3980=EDGE_CURVE('',#3149,#3147,#1971,.T.);
#3981=EDGE_CURVE('',#3150,#3148,#1972,.T.);
#3982=EDGE_CURVE('',#3150,#3151,#1973,.T.);
#3983=EDGE_CURVE('',#3151,#3149,#1974,.T.);
#3984=EDGE_CURVE('',#3141,#3150,#1975,.T.);
#3985=EDGE_CURVE('',#3143,#3151,#1976,.T.);
#3986=EDGE_CURVE('',#3152,#3152,#2772,.T.);
#3987=EDGE_CURVE('',#3152,#3153,#1977,.T.);
#3988=EDGE_CURVE('',#3153,#3153,#2773,.T.);
#3989=EDGE_CURVE('',#3139,#3154,#1978,.T.);
#3990=EDGE_CURVE('',#3154,#3154,#2774,.T.);
#3991=EDGE_CURVE('',#3155,#3156,#1979,.T.);
#3992=EDGE_CURVE('',#3157,#3155,#1980,.T.);
#3993=EDGE_CURVE('',#3158,#3157,#1981,.T.);
#3994=EDGE_CURVE('',#3158,#3156,#1982,.T.);
#3995=EDGE_CURVE('',#3159,#3160,#1983,.T.);
#3996=EDGE_CURVE('',#3159,#3161,#1984,.T.);
#3997=EDGE_CURVE('',#3162,#3161,#1985,.T.);
#3998=EDGE_CURVE('',#3160,#3162,#1986,.T.);
#3999=EDGE_CURVE('',#3163,#3164,#1987,.T.);
#4000=EDGE_CURVE('',#3163,#3165,#1988,.T.);
#4001=EDGE_CURVE('',#3166,#3165,#1989,.T.);
#4002=EDGE_CURVE('',#3164,#3166,#1990,.T.);
#4003=EDGE_CURVE('',#3167,#3168,#1991,.T.);
#4004=EDGE_CURVE('',#3167,#3169,#1992,.T.);
#4005=EDGE_CURVE('',#3170,#3169,#1993,.T.);
#4006=EDGE_CURVE('',#3168,#3170,#1994,.T.);
#4007=EDGE_CURVE('',#3171,#3172,#1995,.T.);
#4008=EDGE_CURVE('',#3171,#3173,#1996,.T.);
#4009=EDGE_CURVE('',#3174,#3173,#1997,.T.);
#4010=EDGE_CURVE('',#3172,#3174,#1998,.T.);
#4011=EDGE_CURVE('',#3175,#3176,#1999,.T.);
#4012=EDGE_CURVE('',#3177,#3175,#2000,.T.);
#4013=EDGE_CURVE('',#3178,#3177,#2001,.T.);
#4014=EDGE_CURVE('',#3178,#3176,#2002,.T.);
#4015=EDGE_CURVE('',#3179,#3180,#2003,.T.);
#4016=EDGE_CURVE('',#3181,#3179,#2004,.T.);
#4017=EDGE_CURVE('',#3182,#3181,#2005,.T.);
#4018=EDGE_CURVE('',#3182,#3180,#2006,.T.);
#4019=EDGE_CURVE('',#3183,#3183,#2775,.T.);
#4020=EDGE_CURVE('',#3184,#3184,#2776,.T.);
#4021=EDGE_CURVE('',#3156,#3171,#2007,.T.);
#4022=EDGE_CURVE('',#3173,#3158,#2008,.T.);
#4023=EDGE_CURVE('',#3176,#3159,#2009,.T.);
#4024=EDGE_CURVE('',#3161,#3178,#2010,.T.);
#4025=EDGE_CURVE('',#3180,#3163,#2011,.T.);
#4026=EDGE_CURVE('',#3165,#3182,#2012,.T.);
#4027=EDGE_CURVE('',#3185,#3167,#2013,.T.);
#4028=EDGE_CURVE('',#3186,#3185,#2014,.T.);
#4029=EDGE_CURVE('',#3169,#3186,#2015,.T.);
#4030=EDGE_CURVE('',#3187,#3185,#2016,.T.);
#4031=EDGE_CURVE('',#3188,#3187,#2017,.T.);
#4032=EDGE_CURVE('',#3186,#3188,#2018,.T.);
#4033=EDGE_CURVE('',#3189,#3190,#2019,.T.);
#4034=EDGE_CURVE('',#3191,#3190,#264,.T.);
#4035=EDGE_CURVE('',#3192,#3191,#265,.T.);
#4036=EDGE_CURVE('',#3193,#3192,#2020,.T.);
#4037=EDGE_CURVE('',#3194,#3193,#266,.T.);
#4038=EDGE_CURVE('',#3189,#3194,#267,.T.);
#4039=EDGE_CURVE('',#3188,#3195,#2021,.T.);
#4040=EDGE_CURVE('',#3196,#3195,#268,.T.);
#4041=EDGE_CURVE('',#3197,#3196,#269,.T.);
#4042=EDGE_CURVE('',#3198,#3197,#2022,.T.);
#4043=EDGE_CURVE('',#3199,#3198,#270,.T.);
#4044=EDGE_CURVE('',#3200,#3199,#271,.T.);
#4045=EDGE_CURVE('',#3200,#3170,#2023,.T.);
#4046=EDGE_CURVE('',#3181,#3201,#2024,.T.);
#4047=EDGE_CURVE('',#3202,#3201,#272,.T.);
#4048=EDGE_CURVE('',#3203,#3202,#273,.T.);
#4049=EDGE_CURVE('',#3204,#3203,#2025,.T.);
#4050=EDGE_CURVE('',#3205,#3204,#274,.T.);
#4051=EDGE_CURVE('',#3206,#3205,#275,.T.);
#4052=EDGE_CURVE('',#3206,#3166,#2026,.T.);
#4053=EDGE_CURVE('',#3177,#3207,#2027,.T.);
#4054=EDGE_CURVE('',#3208,#3207,#276,.T.);
#4055=EDGE_CURVE('',#3209,#3208,#277,.T.);
#4056=EDGE_CURVE('',#3210,#3209,#2028,.T.);
#4057=EDGE_CURVE('',#3211,#3210,#278,.T.);
#4058=EDGE_CURVE('',#3212,#3211,#279,.T.);
#4059=EDGE_CURVE('',#3212,#3162,#2029,.T.);
#4060=EDGE_CURVE('',#3213,#3172,#2030,.T.);
#4061=EDGE_CURVE('',#3213,#3214,#280,.T.);
#4062=EDGE_CURVE('',#3214,#3215,#2031,.T.);
#4063=EDGE_CURVE('',#3215,#3216,#281,.T.);
#4064=EDGE_CURVE('',#3155,#3216,#2032,.T.);
#4065=EDGE_CURVE('',#3200,#3190,#282,.T.);
#4066=EDGE_CURVE('',#3189,#3195,#283,.T.);
#4067=EDGE_CURVE('',#3217,#3187,#2033,.T.);
#4068=EDGE_CURVE('',#3217,#3201,#284,.T.);
#4069=EDGE_CURVE('',#3218,#3179,#2034,.T.);
#4070=EDGE_CURVE('',#3218,#3207,#285,.T.);
#4071=EDGE_CURVE('',#3219,#3175,#2035,.T.);
#4072=EDGE_CURVE('',#3219,#3220,#286,.T.);
#4073=EDGE_CURVE('',#3220,#3213,#287,.T.);
#4074=EDGE_CURVE('',#3174,#3221,#2036,.T.);
#4075=EDGE_CURVE('',#3222,#3221,#288,.T.);
#4076=EDGE_CURVE('',#3222,#3223,#289,.T.);
#4077=EDGE_CURVE('',#3224,#3223,#290,.T.);
#4078=EDGE_CURVE('',#3224,#3225,#2037,.T.);
#4079=EDGE_CURVE('',#3226,#3225,#291,.T.);
#4080=EDGE_CURVE('',#3226,#3227,#292,.T.);
#4081=EDGE_CURVE('',#3228,#3227,#293,.T.);
#4082=EDGE_CURVE('',#3228,#3157,#2038,.T.);
#4083=EDGE_CURVE('',#3216,#3229,#294,.T.);
#4084=EDGE_CURVE('',#3229,#3230,#295,.T.);
#4085=EDGE_CURVE('',#3160,#3230,#2039,.T.);
#4086=EDGE_CURVE('',#3212,#3231,#296,.T.);
#4087=EDGE_CURVE('',#3164,#3231,#2040,.T.);
#4088=EDGE_CURVE('',#3206,#3232,#297,.T.);
#4089=EDGE_CURVE('',#3168,#3232,#2041,.T.);
#4090=EDGE_CURVE('',#3233,#3234,#298,.T.);
#4091=EDGE_CURVE('',#3234,#3235,#299,.T.);
#4092=EDGE_CURVE('',#3235,#3236,#2042,.T.);
#4093=EDGE_CURVE('',#3236,#3237,#300,.T.);
#4094=EDGE_CURVE('',#3237,#3238,#301,.T.);
#4095=EDGE_CURVE('',#3233,#3238,#2043,.T.);
#4096=EDGE_CURVE('',#3239,#3239,#2777,.T.);
#4097=EDGE_CURVE('',#3239,#3184,#2044,.T.);
#4098=EDGE_CURVE('',#3240,#3240,#2778,.T.);
#4099=EDGE_CURVE('',#3240,#3183,#2045,.T.);
#4100=EDGE_CURVE('',#3233,#3241,#302,.T.);
#4101=EDGE_CURVE('',#3242,#3238,#303,.T.);
#4102=EDGE_CURVE('',#3243,#3242,#304,.T.);
#4103=EDGE_CURVE('',#3244,#3243,#2046,.T.);
#4104=EDGE_CURVE('',#3241,#3244,#305,.T.);
#4105=EDGE_CURVE('',#3199,#3191,#306,.T.);
#4106=EDGE_CURVE('',#3241,#3245,#307,.T.);
#4107=EDGE_CURVE('',#3245,#3234,#308,.T.);
#4108=EDGE_CURVE('',#3192,#3198,#309,.T.);
#4109=EDGE_CURVE('',#3246,#3244,#310,.T.);
#4110=EDGE_CURVE('',#3245,#3246,#2779,.F.);
#4111=EDGE_CURVE('',#3197,#3193,#311,.T.);
#4112=EDGE_CURVE('',#3243,#3247,#312,.T.);
#4113=EDGE_CURVE('',#3247,#3246,#2047,.T.);
#4114=EDGE_CURVE('',#3194,#3196,#313,.T.);
#4115=EDGE_CURVE('',#3237,#3248,#314,.T.);
#4116=EDGE_CURVE('',#3248,#3242,#315,.T.);
#4117=EDGE_CURVE('',#3249,#3232,#316,.T.);
#4118=EDGE_CURVE('',#3250,#3249,#317,.T.);
#4119=EDGE_CURVE('',#3251,#3250,#2048,.T.);
#4120=EDGE_CURVE('',#3252,#3251,#318,.T.);
#4121=EDGE_CURVE('',#3217,#3252,#319,.T.);
#4122=EDGE_CURVE('',#3205,#3249,#320,.T.);
#4123=EDGE_CURVE('',#3250,#3204,#321,.T.);
#4124=EDGE_CURVE('',#3203,#3251,#322,.T.);
#4125=EDGE_CURVE('',#3252,#3202,#323,.T.);
#4126=EDGE_CURVE('',#3253,#3231,#324,.T.);
#4127=EDGE_CURVE('',#3254,#3253,#325,.T.);
#4128=EDGE_CURVE('',#3255,#3254,#2049,.T.);
#4129=EDGE_CURVE('',#3256,#3255,#326,.T.);
#4130=EDGE_CURVE('',#3218,#3256,#327,.T.);
#4131=EDGE_CURVE('',#3211,#3253,#328,.T.);
#4132=EDGE_CURVE('',#3254,#3210,#329,.T.);
#4133=EDGE_CURVE('',#3209,#3255,#330,.T.);
#4134=EDGE_CURVE('',#3256,#3208,#331,.T.);
#4135=EDGE_CURVE('',#3257,#3230,#332,.T.);
#4136=EDGE_CURVE('',#3258,#3257,#333,.T.);
#4137=EDGE_CURVE('',#3259,#3258,#2050,.T.);
#4138=EDGE_CURVE('',#3260,#3259,#334,.T.);
#4139=EDGE_CURVE('',#3219,#3260,#335,.T.);
#4140=EDGE_CURVE('',#3229,#3261,#336,.T.);
#4141=EDGE_CURVE('',#3261,#3257,#337,.T.);
#4142=EDGE_CURVE('',#3262,#3261,#2780,.F.);
#4143=EDGE_CURVE('',#3258,#3262,#338,.T.);
#4144=EDGE_CURVE('',#3262,#3263,#2051,.T.);
#4145=EDGE_CURVE('',#3263,#3259,#339,.T.);
#4146=EDGE_CURVE('',#3260,#3264,#340,.T.);
#4147=EDGE_CURVE('',#3264,#3220,#341,.T.);
#4148=EDGE_CURVE('',#3264,#3263,#2781,.F.);
#4149=EDGE_CURVE('',#3263,#3214,#2782,.F.);
#4150=EDGE_CURVE('',#3214,#3264,#2783,.F.);
#4151=EDGE_CURVE('',#3247,#3248,#2784,.F.);
#4152=EDGE_CURVE('',#3248,#3265,#2785,.F.);
#4153=EDGE_CURVE('',#3265,#3247,#2786,.F.);
#4154=EDGE_CURVE('',#3261,#3215,#2787,.F.);
#4155=EDGE_CURVE('',#3215,#3262,#2788,.F.);
#4156=EDGE_CURVE('',#3266,#3245,#2789,.F.);
#4157=EDGE_CURVE('',#3246,#3266,#2790,.F.);
#4158=EDGE_CURVE('',#3266,#3265,#2052,.T.);
#4159=EDGE_CURVE('',#3235,#3266,#342,.T.);
#4160=EDGE_CURVE('',#3265,#3236,#343,.T.);
#4161=EDGE_CURVE('',#3267,#3268,#2791,.F.);
#4162=EDGE_CURVE('',#3269,#3267,#2792,.F.);
#4163=EDGE_CURVE('',#3268,#3269,#2793,.F.);
#4164=EDGE_CURVE('',#3270,#3271,#2794,.F.);
#4165=EDGE_CURVE('',#3272,#3270,#2795,.F.);
#4166=EDGE_CURVE('',#3271,#3272,#2796,.F.);
#4167=EDGE_CURVE('',#3273,#3274,#2797,.F.);
#4168=EDGE_CURVE('',#3275,#3273,#2798,.F.);
#4169=EDGE_CURVE('',#3274,#3275,#2799,.F.);
#4170=EDGE_CURVE('',#3268,#3275,#2053,.T.);
#4171=EDGE_CURVE('',#3273,#3267,#2054,.T.);
#4172=EDGE_CURVE('',#3227,#3274,#344,.T.);
#4173=EDGE_CURVE('',#3275,#3228,#345,.T.);
#4174=EDGE_CURVE('',#3276,#3277,#2800,.F.);
#4175=EDGE_CURVE('',#3278,#3276,#2801,.F.);
#4176=EDGE_CURVE('',#3277,#3278,#2802,.F.);
#4177=EDGE_CURVE('',#3276,#3272,#2055,.T.);
#4178=EDGE_CURVE('',#3270,#3278,#2056,.T.);
#4179=EDGE_CURVE('',#3274,#3277,#346,.T.);
#4180=EDGE_CURVE('',#3278,#3273,#347,.T.);
#4181=EDGE_CURVE('',#3225,#3276,#348,.T.);
#4182=EDGE_CURVE('',#3277,#3226,#349,.T.);
#4183=EDGE_CURVE('',#3223,#3271,#350,.T.);
#4184=EDGE_CURVE('',#3272,#3224,#351,.T.);
#4185=EDGE_CURVE('',#3271,#3269,#352,.T.);
#4186=EDGE_CURVE('',#3267,#3270,#353,.T.);
#4187=EDGE_CURVE('',#3221,#3268,#354,.T.);
#4188=EDGE_CURVE('',#3269,#3222,#355,.T.);
#4189=EDGE_CURVE('',#3279,#3279,#2803,.T.);
#4190=EDGE_CURVE('',#3279,#3280,#2057,.T.);
#4191=EDGE_CURVE('',#3280,#3280,#2804,.T.);
#4192=EDGE_CURVE('',#3281,#3281,#2805,.T.);
#4193=EDGE_CURVE('',#3281,#3282,#2058,.T.);
#4194=EDGE_CURVE('',#3282,#3282,#2806,.T.);
#4195=EDGE_CURVE('',#3283,#3283,#2807,.T.);
#4196=EDGE_CURVE('',#3284,#3284,#2808,.T.);
#4197=EDGE_CURVE('',#3285,#3285,#2809,.T.);
#4198=EDGE_CURVE('',#3285,#3283,#2059,.T.);
#4199=EDGE_CURVE('',#3286,#3286,#2810,.T.);
#4200=EDGE_CURVE('',#3287,#3287,#2811,.T.);
#4201=EDGE_CURVE('',#3288,#3288,#2812,.T.);
#4202=EDGE_CURVE('',#3288,#3286,#2060,.T.);
#4203=EDGE_CURVE('',#3289,#3289,#2813,.T.);
#4204=EDGE_CURVE('',#3290,#3290,#2814,.T.);
#4205=EDGE_CURVE('',#3291,#3291,#2815,.T.);
#4206=EDGE_CURVE('',#3291,#3289,#2061,.T.);
#4207=EDGE_CURVE('',#3292,#3292,#2816,.T.);
#4208=EDGE_CURVE('',#3293,#3293,#2817,.T.);
#4209=EDGE_CURVE('',#3294,#3294,#2818,.T.);
#4210=EDGE_CURVE('',#3294,#3292,#2062,.T.);
#4211=EDGE_CURVE('',#3284,#3295,#2063,.T.);
#4212=EDGE_CURVE('',#3295,#3295,#2819,.T.);
#4213=EDGE_CURVE('',#3287,#3296,#2064,.T.);
#4214=EDGE_CURVE('',#3296,#3296,#2820,.T.);
#4215=EDGE_CURVE('',#3290,#3297,#2065,.T.);
#4216=EDGE_CURVE('',#3297,#3297,#2821,.T.);
#4217=EDGE_CURVE('',#3293,#3298,#2066,.T.);
#4218=EDGE_CURVE('',#3298,#3298,#2822,.T.);
#4219=EDGE_CURVE('',#3299,#3300,#2823,.T.);
#4220=EDGE_CURVE('',#3300,#3301,#356,.T.);
#4221=EDGE_CURVE('',#3301,#3302,#2824,.T.);
#4222=EDGE_CURVE('',#3302,#3299,#357,.T.);
#4223=EDGE_CURVE('',#3303,#3304,#2825,.T.);
#4224=EDGE_CURVE('',#3304,#3300,#2067,.T.);
#4225=EDGE_CURVE('',#3299,#3303,#2068,.T.);
#4226=EDGE_CURVE('',#3305,#3306,#2826,.T.);
#4227=EDGE_CURVE('',#3306,#3304,#358,.T.);
#4228=EDGE_CURVE('',#3303,#3305,#359,.T.);
#4229=EDGE_CURVE('',#3307,#3308,#2827,.T.);
#4230=EDGE_CURVE('',#3308,#3306,#360,.T.);
#4231=EDGE_CURVE('',#3305,#3307,#361,.T.);
#4232=EDGE_CURVE('',#3309,#3310,#2828,.T.);
#4233=EDGE_CURVE('',#3310,#3308,#362,.T.);
#4234=EDGE_CURVE('',#3307,#3309,#363,.T.);
#4235=EDGE_CURVE('',#3311,#3312,#2829,.T.);
#4236=EDGE_CURVE('',#3312,#3310,#2069,.T.);
#4237=EDGE_CURVE('',#3309,#3311,#2070,.T.);
#4238=EDGE_CURVE('',#3313,#3314,#2830,.T.);
#4239=EDGE_CURVE('',#3314,#3312,#364,.T.);
#4240=EDGE_CURVE('',#3311,#3313,#365,.T.);
#4241=EDGE_CURVE('',#3301,#3314,#366,.T.);
#4242=EDGE_CURVE('',#3313,#3302,#367,.T.);
#4243=EDGE_CURVE('',#3315,#3312,#368,.T.);
#4244=EDGE_CURVE('',#3316,#3315,#2071,.T.);
#4245=EDGE_CURVE('',#3310,#3316,#369,.T.);
#4246=EDGE_CURVE('',#3314,#3317,#370,.T.);
#4247=EDGE_CURVE('',#3317,#3315,#371,.T.);
#4248=EDGE_CURVE('',#3318,#3301,#372,.T.);
#4249=EDGE_CURVE('',#3317,#3318,#373,.T.);
#4250=EDGE_CURVE('',#3300,#3319,#374,.T.);
#4251=EDGE_CURVE('',#3319,#3318,#375,.T.);
#4252=EDGE_CURVE('',#3320,#3304,#376,.T.);
#4253=EDGE_CURVE('',#3319,#3320,#2072,.T.);
#4254=EDGE_CURVE('',#3316,#3321,#377,.T.);
#4255=EDGE_CURVE('',#3321,#3308,#378,.T.);
#4256=EDGE_CURVE('',#3306,#3322,#379,.T.);
#4257=EDGE_CURVE('',#3322,#3320,#380,.T.);
#4258=EDGE_CURVE('',#3322,#3321,#381,.T.);
#4259=EDGE_CURVE('',#3323,#3324,#2073,.T.);
#4260=EDGE_CURVE('',#3323,#3325,#382,.T.);
#4261=EDGE_CURVE('',#3325,#3326,#2831,.F.);
#4262=EDGE_CURVE('',#3326,#3324,#383,.T.);
#4263=EDGE_CURVE('',#3327,#3328,#2074,.T.);
#4264=EDGE_CURVE('',#3327,#3323,#384,.T.);
#4265=EDGE_CURVE('',#3324,#3328,#385,.T.);
#4266=EDGE_CURVE('',#3329,#3330,#2075,.T.);
#4267=EDGE_CURVE('',#3329,#3327,#386,.T.);
#4268=EDGE_CURVE('',#3328,#3330,#387,.T.);
#4269=EDGE_CURVE('',#3331,#3332,#2076,.T.);
#4270=EDGE_CURVE('',#3331,#3329,#388,.T.);
#4271=EDGE_CURVE('',#3330,#3332,#389,.T.);
#4272=EDGE_CURVE('',#3333,#3334,#2077,.T.);
#4273=EDGE_CURVE('',#3333,#3331,#390,.T.);
#4274=EDGE_CURVE('',#3332,#3334,#391,.T.);
#4275=EDGE_CURVE('',#3335,#3336,#2078,.T.);
#4276=EDGE_CURVE('',#3335,#3333,#392,.T.);
#4277=EDGE_CURVE('',#3334,#3336,#393,.T.);
#4278=EDGE_CURVE('',#3337,#3338,#2079,.T.);
#4279=EDGE_CURVE('',#3337,#3335,#394,.T.);
#4280=EDGE_CURVE('',#3336,#3338,#395,.T.);
#4281=EDGE_CURVE('',#3339,#3340,#2080,.T.);
#4282=EDGE_CURVE('',#3339,#3337,#396,.T.);
#4283=EDGE_CURVE('',#3338,#3340,#397,.T.);
#4284=EDGE_CURVE('',#3341,#3342,#2081,.T.);
#4285=EDGE_CURVE('',#3341,#3339,#398,.T.);
#4286=EDGE_CURVE('',#3340,#3342,#399,.T.);
#4287=EDGE_CURVE('',#3343,#3344,#2082,.T.);
#4288=EDGE_CURVE('',#3343,#3341,#400,.T.);
#4289=EDGE_CURVE('',#3342,#3344,#401,.T.);
#4290=EDGE_CURVE('',#3345,#3346,#2083,.T.);
#4291=EDGE_CURVE('',#3345,#3343,#402,.T.);
#4292=EDGE_CURVE('',#3344,#3346,#403,.T.);
#4293=EDGE_CURVE('',#3347,#3348,#2084,.T.);
#4294=EDGE_CURVE('',#3347,#3345,#404,.T.);
#4295=EDGE_CURVE('',#3346,#3348,#405,.T.);
#4296=EDGE_CURVE('',#3349,#3350,#2085,.T.);
#4297=EDGE_CURVE('',#3349,#3347,#406,.T.);
#4298=EDGE_CURVE('',#3348,#3350,#407,.T.);
#4299=EDGE_CURVE('',#3351,#3352,#2086,.T.);
#4300=EDGE_CURVE('',#3351,#3349,#408,.T.);
#4301=EDGE_CURVE('',#3350,#3352,#409,.T.);
#4302=EDGE_CURVE('',#3353,#3354,#2087,.T.);
#4303=EDGE_CURVE('',#3353,#3351,#410,.T.);
#4304=EDGE_CURVE('',#3352,#3354,#411,.T.);
#4305=EDGE_CURVE('',#3355,#3356,#2088,.T.);
#4306=EDGE_CURVE('',#3355,#3353,#412,.T.);
#4307=EDGE_CURVE('',#3354,#3356,#413,.T.);
#4308=EDGE_CURVE('',#3357,#3358,#2089,.T.);
#4309=EDGE_CURVE('',#3357,#3355,#414,.T.);
#4310=EDGE_CURVE('',#3356,#3358,#415,.T.);
#4311=EDGE_CURVE('',#3359,#3360,#2090,.T.);
#4312=EDGE_CURVE('',#3359,#3357,#416,.T.);
#4313=EDGE_CURVE('',#3358,#3360,#417,.T.);
#4314=EDGE_CURVE('',#3361,#3362,#2091,.T.);
#4315=EDGE_CURVE('',#3361,#3359,#418,.T.);
#4316=EDGE_CURVE('',#3360,#3362,#419,.T.);
#4317=EDGE_CURVE('',#3363,#3364,#2092,.T.);
#4318=EDGE_CURVE('',#3363,#3361,#420,.T.);
#4319=EDGE_CURVE('',#3362,#3364,#421,.T.);
#4320=EDGE_CURVE('',#3365,#3366,#2093,.T.);
#4321=EDGE_CURVE('',#3365,#3363,#422,.T.);
#4322=EDGE_CURVE('',#3364,#3366,#423,.T.);
#4323=EDGE_CURVE('',#3367,#3368,#2094,.T.);
#4324=EDGE_CURVE('',#3367,#3365,#424,.T.);
#4325=EDGE_CURVE('',#3366,#3368,#425,.T.);
#4326=EDGE_CURVE('',#3369,#3370,#2095,.T.);
#4327=EDGE_CURVE('',#3369,#3367,#426,.T.);
#4328=EDGE_CURVE('',#3368,#3370,#427,.T.);
#4329=EDGE_CURVE('',#3371,#3372,#2096,.T.);
#4330=EDGE_CURVE('',#3371,#3369,#428,.T.);
#4331=EDGE_CURVE('',#3370,#3372,#429,.T.);
#4332=EDGE_CURVE('',#3373,#3374,#2097,.T.);
#4333=EDGE_CURVE('',#3373,#3371,#430,.T.);
#4334=EDGE_CURVE('',#3372,#3374,#431,.T.);
#4335=EDGE_CURVE('',#3375,#3376,#2098,.T.);
#4336=EDGE_CURVE('',#3375,#3373,#432,.T.);
#4337=EDGE_CURVE('',#3374,#3376,#433,.T.);
#4338=EDGE_CURVE('',#3377,#3378,#2099,.T.);
#4339=EDGE_CURVE('',#3377,#3375,#434,.T.);
#4340=EDGE_CURVE('',#3376,#3378,#435,.T.);
#4341=EDGE_CURVE('',#3379,#3380,#2100,.T.);
#4342=EDGE_CURVE('',#3379,#3377,#436,.T.);
#4343=EDGE_CURVE('',#3378,#3380,#437,.T.);
#4344=EDGE_CURVE('',#3381,#3382,#2101,.T.);
#4345=EDGE_CURVE('',#3381,#3379,#438,.T.);
#4346=EDGE_CURVE('',#3380,#3382,#439,.T.);
#4347=EDGE_CURVE('',#3383,#3384,#2102,.T.);
#4348=EDGE_CURVE('',#3383,#3381,#440,.T.);
#4349=EDGE_CURVE('',#3382,#3384,#441,.T.);
#4350=EDGE_CURVE('',#3385,#3386,#2103,.T.);
#4351=EDGE_CURVE('',#3385,#3387,#442,.T.);
#4352=EDGE_CURVE('',#3387,#3388,#2832,.T.);
#4353=EDGE_CURVE('',#3386,#3388,#443,.T.);
#4354=EDGE_CURVE('',#3389,#3390,#2104,.T.);
#4355=EDGE_CURVE('',#3389,#3385,#444,.T.);
#4356=EDGE_CURVE('',#3390,#3386,#445,.T.);
#4357=EDGE_CURVE('',#3391,#3392,#2105,.T.);
#4358=EDGE_CURVE('',#3391,#3389,#446,.T.);
#4359=EDGE_CURVE('',#3392,#3390,#447,.T.);
#4360=EDGE_CURVE('',#3393,#3394,#2106,.T.);
#4361=EDGE_CURVE('',#3393,#3391,#448,.T.);
#4362=EDGE_CURVE('',#3394,#3392,#449,.T.);
#4363=EDGE_CURVE('',#3395,#3396,#2107,.T.);
#4364=EDGE_CURVE('',#3395,#3393,#450,.T.);
#4365=EDGE_CURVE('',#3396,#3394,#451,.T.);
#4366=EDGE_CURVE('',#3397,#3398,#2108,.T.);
#4367=EDGE_CURVE('',#3397,#3395,#452,.T.);
#4368=EDGE_CURVE('',#3398,#3396,#453,.T.);
#4369=EDGE_CURVE('',#3399,#3400,#2109,.T.);
#4370=EDGE_CURVE('',#3399,#3397,#454,.T.);
#4371=EDGE_CURVE('',#3400,#3398,#455,.T.);
#4372=EDGE_CURVE('',#3401,#3402,#2110,.T.);
#4373=EDGE_CURVE('',#3401,#3399,#456,.T.);
#4374=EDGE_CURVE('',#3402,#3400,#457,.T.);
#4375=EDGE_CURVE('',#3403,#3404,#2111,.T.);
#4376=EDGE_CURVE('',#3403,#3401,#458,.T.);
#4377=EDGE_CURVE('',#3404,#3402,#459,.T.);
#4378=EDGE_CURVE('',#3405,#3406,#2112,.T.);
#4379=EDGE_CURVE('',#3405,#3403,#460,.T.);
#4380=EDGE_CURVE('',#3406,#3404,#461,.T.);
#4381=EDGE_CURVE('',#3407,#3408,#2113,.T.);
#4382=EDGE_CURVE('',#3407,#3405,#462,.T.);
#4383=EDGE_CURVE('',#3408,#3406,#463,.T.);
#4384=EDGE_CURVE('',#3409,#3410,#2114,.T.);
#4385=EDGE_CURVE('',#3409,#3407,#464,.T.);
#4386=EDGE_CURVE('',#3410,#3408,#465,.T.);
#4387=EDGE_CURVE('',#3411,#3412,#2115,.T.);
#4388=EDGE_CURVE('',#3411,#3409,#466,.T.);
#4389=EDGE_CURVE('',#3412,#3410,#467,.T.);
#4390=EDGE_CURVE('',#3413,#3414,#2116,.T.);
#4391=EDGE_CURVE('',#3413,#3411,#468,.T.);
#4392=EDGE_CURVE('',#3414,#3412,#469,.T.);
#4393=EDGE_CURVE('',#3415,#3416,#2117,.T.);
#4394=EDGE_CURVE('',#3415,#3413,#470,.T.);
#4395=EDGE_CURVE('',#3416,#3414,#471,.T.);
#4396=EDGE_CURVE('',#3417,#3418,#2118,.T.);
#4397=EDGE_CURVE('',#3417,#3415,#472,.T.);
#4398=EDGE_CURVE('',#3418,#3416,#473,.T.);
#4399=EDGE_CURVE('',#3419,#3420,#2119,.T.);
#4400=EDGE_CURVE('',#3419,#3417,#474,.T.);
#4401=EDGE_CURVE('',#3420,#3418,#475,.T.);
#4402=EDGE_CURVE('',#3421,#3422,#2120,.T.);
#4403=EDGE_CURVE('',#3421,#3419,#476,.T.);
#4404=EDGE_CURVE('',#3422,#3420,#477,.T.);
#4405=EDGE_CURVE('',#3423,#3424,#2121,.T.);
#4406=EDGE_CURVE('',#3423,#3421,#478,.T.);
#4407=EDGE_CURVE('',#3424,#3422,#479,.T.);
#4408=EDGE_CURVE('',#3425,#3426,#2122,.T.);
#4409=EDGE_CURVE('',#3425,#3423,#480,.T.);
#4410=EDGE_CURVE('',#3426,#3424,#481,.T.);
#4411=EDGE_CURVE('',#3427,#3428,#2123,.T.);
#4412=EDGE_CURVE('',#3427,#3425,#482,.T.);
#4413=EDGE_CURVE('',#3428,#3426,#483,.T.);
#4414=EDGE_CURVE('',#3429,#3430,#2124,.T.);
#4415=EDGE_CURVE('',#3429,#3427,#484,.T.);
#4416=EDGE_CURVE('',#3430,#3428,#485,.T.);
#4417=EDGE_CURVE('',#3431,#3432,#2125,.T.);
#4418=EDGE_CURVE('',#3431,#3429,#486,.T.);
#4419=EDGE_CURVE('',#3432,#3430,#487,.T.);
#4420=EDGE_CURVE('',#3433,#3434,#2126,.T.);
#4421=EDGE_CURVE('',#3433,#3431,#488,.T.);
#4422=EDGE_CURVE('',#3434,#3432,#489,.T.);
#4423=EDGE_CURVE('',#3435,#3436,#2127,.T.);
#4424=EDGE_CURVE('',#3435,#3433,#490,.T.);
#4425=EDGE_CURVE('',#3436,#3434,#491,.T.);
#4426=EDGE_CURVE('',#3437,#3438,#2128,.T.);
#4427=EDGE_CURVE('',#3437,#3435,#492,.T.);
#4428=EDGE_CURVE('',#3438,#3436,#493,.T.);
#4429=EDGE_CURVE('',#3439,#3440,#2129,.T.);
#4430=EDGE_CURVE('',#3439,#3437,#494,.T.);
#4431=EDGE_CURVE('',#3440,#3438,#495,.T.);
#4432=EDGE_CURVE('',#3441,#3442,#2130,.T.);
#4433=EDGE_CURVE('',#3441,#3439,#496,.T.);
#4434=EDGE_CURVE('',#3442,#3440,#497,.T.);
#4435=EDGE_CURVE('',#3443,#3444,#2131,.T.);
#4436=EDGE_CURVE('',#3443,#3441,#498,.T.);
#4437=EDGE_CURVE('',#3444,#3442,#499,.T.);
#4438=EDGE_CURVE('',#3445,#3446,#2132,.T.);
#4439=EDGE_CURVE('',#3445,#3443,#500,.T.);
#4440=EDGE_CURVE('',#3446,#3444,#501,.T.);
#4441=EDGE_CURVE('',#3388,#3447,#502,.T.);
#4442=EDGE_CURVE('',#3448,#3387,#503,.T.);
#4443=EDGE_CURVE('',#3449,#3448,#2833,.T.);
#4444=EDGE_CURVE('',#3447,#3449,#504,.T.);
#4445=EDGE_CURVE('',#3447,#3450,#2133,.T.);
#4446=EDGE_CURVE('',#3450,#3450,#2834,.T.);
#4447=EDGE_CURVE('',#3451,#3445,#505,.T.);
#4448=EDGE_CURVE('',#3325,#3451,#506,.T.);
#4449=EDGE_CURVE('',#3448,#3383,#507,.T.);
#4450=EDGE_CURVE('',#3452,#3446,#508,.T.);
#4451=EDGE_CURVE('',#3451,#3452,#2835,.T.);
#4452=EDGE_CURVE('',#3384,#3449,#509,.T.);
#4453=EDGE_CURVE('',#3452,#3326,#510,.T.);
#4454=EDGE_CURVE('',#3453,#3454,#2134,.T.);
#4455=EDGE_CURVE('',#3453,#3455,#2135,.T.);
#4456=EDGE_CURVE('',#3455,#3456,#2136,.T.);
#4457=EDGE_CURVE('',#3454,#3456,#2137,.T.);
#4458=EDGE_CURVE('',#3457,#3453,#2138,.T.);
#4459=EDGE_CURVE('',#3457,#3458,#2139,.T.);
#4460=EDGE_CURVE('',#3458,#3455,#2140,.T.);
#4461=EDGE_CURVE('',#3459,#3457,#2141,.T.);
#4462=EDGE_CURVE('',#3459,#3460,#2142,.T.);
#4463=EDGE_CURVE('',#3460,#3458,#2143,.T.);
#4464=EDGE_CURVE('',#3461,#3459,#2144,.T.);
#4465=EDGE_CURVE('',#3461,#3462,#2145,.T.);
#4466=EDGE_CURVE('',#3462,#3460,#2146,.T.);
#4467=EDGE_CURVE('',#3463,#3461,#2147,.T.);
#4468=EDGE_CURVE('',#3463,#3464,#2148,.T.);
#4469=EDGE_CURVE('',#3464,#3462,#2149,.T.);
#4470=EDGE_CURVE('',#3454,#3463,#2150,.T.);
#4471=EDGE_CURVE('',#3456,#3464,#2151,.T.);
#4472=EDGE_CURVE('',#3465,#3465,#2836,.T.);
#4473=EDGE_CURVE('',#3465,#3466,#2152,.T.);
#4474=EDGE_CURVE('',#3466,#3466,#2837,.T.);
#4475=EDGE_CURVE('',#3467,#3468,#2153,.T.);
#4476=EDGE_CURVE('',#3469,#3468,#2838,.F.);
#4477=EDGE_CURVE('',#3469,#3467,#511,.T.);
#4478=EDGE_CURVE('',#3470,#3471,#2154,.T.);
#4479=EDGE_CURVE('',#3471,#3472,#512,.T.);
#4480=EDGE_CURVE('',#3468,#3472,#2839,.F.);
#4481=EDGE_CURVE('',#3467,#3470,#513,.T.);
#4482=EDGE_CURVE('',#3473,#3474,#2155,.T.);
#4483=EDGE_CURVE('',#3474,#3471,#514,.T.);
#4484=EDGE_CURVE('',#3470,#3473,#515,.T.);
#4485=EDGE_CURVE('',#3475,#3476,#2156,.T.);
#4486=EDGE_CURVE('',#3476,#3474,#516,.T.);
#4487=EDGE_CURVE('',#3473,#3475,#517,.T.);
#4488=EDGE_CURVE('',#3477,#3478,#2157,.T.);
#4489=EDGE_CURVE('',#3477,#3479,#518,.T.);
#4490=EDGE_CURVE('',#3480,#3479,#2840,.T.);
#4491=EDGE_CURVE('',#3480,#3478,#519,.T.);
#4492=EDGE_CURVE('',#3481,#3482,#2158,.T.);
#4493=EDGE_CURVE('',#3482,#3483,#520,.T.);
#4494=EDGE_CURVE('',#3484,#3483,#2841,.T.);
#4495=EDGE_CURVE('',#3481,#3484,#521,.T.);
#4496=EDGE_CURVE('',#3485,#3486,#2159,.T.);
#4497=EDGE_CURVE('',#3486,#3482,#522,.T.);
#4498=EDGE_CURVE('',#3485,#3481,#523,.T.);
#4499=EDGE_CURVE('',#3487,#3488,#2160,.T.);
#4500=EDGE_CURVE('',#3488,#3486,#524,.T.);
#4501=EDGE_CURVE('',#3487,#3485,#525,.T.);
#4502=EDGE_CURVE('',#3489,#3490,#2161,.T.);
#4503=EDGE_CURVE('',#3490,#3488,#526,.T.);
#4504=EDGE_CURVE('',#3489,#3487,#527,.T.);
#4505=EDGE_CURVE('',#3491,#3492,#2162,.T.);
#4506=EDGE_CURVE('',#3493,#3491,#528,.T.);
#4507=EDGE_CURVE('',#3494,#3493,#2842,.T.);
#4508=EDGE_CURVE('',#3494,#3492,#529,.T.);
#4509=EDGE_CURVE('',#3492,#3490,#530,.T.);
#4510=EDGE_CURVE('',#3491,#3489,#531,.T.);
#4511=EDGE_CURVE('',#3483,#3469,#532,.T.);
#4512=EDGE_CURVE('',#3479,#3494,#533,.T.);
#4513=EDGE_CURVE('',#3475,#3477,#534,.T.);
#4514=EDGE_CURVE('',#3472,#3484,#535,.T.);
#4515=EDGE_CURVE('',#3478,#3476,#536,.T.);
#4516=EDGE_CURVE('',#3493,#3480,#537,.T.);
#4517=EDGE_CURVE('',#3495,#3496,#2163,.T.);
#4518=EDGE_CURVE('',#3496,#3497,#2164,.T.);
#4519=EDGE_CURVE('',#3497,#3498,#2165,.T.);
#4520=EDGE_CURVE('',#3498,#3499,#2166,.T.);
#4521=EDGE_CURVE('',#3499,#3500,#2167,.T.);
#4522=EDGE_CURVE('',#3500,#3495,#2168,.T.);
#4523=EDGE_CURVE('',#3501,#3502,#2169,.T.);
#4524=EDGE_CURVE('',#3502,#3495,#2170,.T.);
#4525=EDGE_CURVE('',#3501,#3500,#2171,.T.);
#4526=EDGE_CURVE('',#3503,#3501,#2172,.T.);
#4527=EDGE_CURVE('',#3503,#3499,#2173,.T.);
#4528=EDGE_CURVE('',#3504,#3503,#2174,.T.);
#4529=EDGE_CURVE('',#3504,#3498,#2175,.T.);
#4530=EDGE_CURVE('',#3505,#3504,#2176,.T.);
#4531=EDGE_CURVE('',#3505,#3497,#2177,.T.);
#4532=EDGE_CURVE('',#3506,#3505,#2178,.T.);
#4533=EDGE_CURVE('',#3506,#3496,#2179,.T.);
#4534=EDGE_CURVE('',#3502,#3506,#2180,.T.);
#4535=EDGE_CURVE('',#3507,#3507,#2843,.T.);
#4536=EDGE_CURVE('',#3507,#3508,#2181,.T.);
#4537=EDGE_CURVE('',#3508,#3508,#2844,.T.);
#4538=EDGE_CURVE('',#3509,#3509,#2845,.T.);
#4539=EDGE_CURVE('',#3509,#3510,#2182,.T.);
#4540=EDGE_CURVE('',#3510,#3510,#2846,.T.);
#4541=ORIENTED_EDGE('',*,*,#3511,.F.);
#4542=ORIENTED_EDGE('',*,*,#3512,.T.);
#4543=ORIENTED_EDGE('',*,*,#3513,.F.);
#4544=ORIENTED_EDGE('',*,*,#3512,.F.);
#4545=ORIENTED_EDGE('',*,*,#3514,.F.);
#4546=ORIENTED_EDGE('',*,*,#3515,.T.);
#4547=ORIENTED_EDGE('',*,*,#3516,.F.);
#4548=ORIENTED_EDGE('',*,*,#3515,.F.);
#4549=ORIENTED_EDGE('',*,*,#3517,.F.);
#4550=ORIENTED_EDGE('',*,*,#3518,.T.);
#4551=ORIENTED_EDGE('',*,*,#3519,.F.);
#4552=ORIENTED_EDGE('',*,*,#3518,.F.);
#4553=ORIENTED_EDGE('',*,*,#3520,.F.);
#4554=ORIENTED_EDGE('',*,*,#3521,.F.);
#4555=ORIENTED_EDGE('',*,*,#3522,.T.);
#4556=ORIENTED_EDGE('',*,*,#3523,.F.);
#4557=ORIENTED_EDGE('',*,*,#3524,.F.);
#4558=ORIENTED_EDGE('',*,*,#3521,.T.);
#4559=ORIENTED_EDGE('',*,*,#3525,.F.);
#4560=ORIENTED_EDGE('',*,*,#3526,.F.);
#4561=ORIENTED_EDGE('',*,*,#3527,.F.);
#4562=ORIENTED_EDGE('',*,*,#3523,.T.);
#4563=ORIENTED_EDGE('',*,*,#3525,.T.);
#4564=ORIENTED_EDGE('',*,*,#3520,.T.);
#4565=ORIENTED_EDGE('',*,*,#3528,.T.);
#4566=ORIENTED_EDGE('',*,*,#3529,.T.);
#4567=ORIENTED_EDGE('',*,*,#3530,.T.);
#4568=ORIENTED_EDGE('',*,*,#3531,.T.);
#4569=ORIENTED_EDGE('',*,*,#3532,.T.);
#4570=ORIENTED_EDGE('',*,*,#3533,.T.);
#4571=ORIENTED_EDGE('',*,*,#3534,.F.);
#4572=ORIENTED_EDGE('',*,*,#3528,.F.);
#4573=ORIENTED_EDGE('',*,*,#3522,.F.);
#4574=ORIENTED_EDGE('',*,*,#3535,.F.);
#4575=ORIENTED_EDGE('',*,*,#3536,.T.);
#4576=ORIENTED_EDGE('',*,*,#3527,.T.);
#4577=ORIENTED_EDGE('',*,*,#3537,.F.);
#4578=ORIENTED_EDGE('',*,*,#3538,.F.);
#4579=ORIENTED_EDGE('',*,*,#3539,.T.);
#4580=ORIENTED_EDGE('',*,*,#3538,.T.);
#4581=ORIENTED_EDGE('',*,*,#3533,.F.);
#4582=ORIENTED_EDGE('',*,*,#3540,.F.);
#4583=ORIENTED_EDGE('',*,*,#3541,.F.);
#4584=ORIENTED_EDGE('',*,*,#3535,.T.);
#4585=ORIENTED_EDGE('',*,*,#3524,.T.);
#4586=ORIENTED_EDGE('',*,*,#3536,.F.);
#4587=ORIENTED_EDGE('',*,*,#3539,.F.);
#4588=ORIENTED_EDGE('',*,*,#3542,.T.);
#4589=ORIENTED_EDGE('',*,*,#3534,.T.);
#4590=ORIENTED_EDGE('',*,*,#3541,.T.);
#4591=ORIENTED_EDGE('',*,*,#3543,.F.);
#4592=ORIENTED_EDGE('',*,*,#3544,.F.);
#4593=ORIENTED_EDGE('',*,*,#3545,.T.);
#4594=ORIENTED_EDGE('',*,*,#3529,.F.);
#4595=ORIENTED_EDGE('',*,*,#3546,.F.);
#4596=ORIENTED_EDGE('',*,*,#3547,.F.);
#4597=ORIENTED_EDGE('',*,*,#3548,.F.);
#4598=ORIENTED_EDGE('',*,*,#3549,.F.);
#4599=ORIENTED_EDGE('',*,*,#3543,.T.);
#4600=ORIENTED_EDGE('',*,*,#3542,.F.);
#4601=ORIENTED_EDGE('',*,*,#3540,.T.);
#4602=ORIENTED_EDGE('',*,*,#3532,.F.);
#4603=ORIENTED_EDGE('',*,*,#3531,.F.);
#4604=ORIENTED_EDGE('',*,*,#3550,.F.);
#4605=ORIENTED_EDGE('',*,*,#3551,.F.);
#4606=ORIENTED_EDGE('',*,*,#3546,.T.);
#4607=ORIENTED_EDGE('',*,*,#3526,.T.);
#4608=ORIENTED_EDGE('',*,*,#3537,.T.);
#4609=ORIENTED_EDGE('',*,*,#3552,.F.);
#4610=ORIENTED_EDGE('',*,*,#3553,.F.);
#4611=ORIENTED_EDGE('',*,*,#3554,.F.);
#4612=ORIENTED_EDGE('',*,*,#3550,.T.);
#4613=ORIENTED_EDGE('',*,*,#3530,.F.);
#4614=ORIENTED_EDGE('',*,*,#3545,.F.);
#4615=ORIENTED_EDGE('',*,*,#3549,.T.);
#4616=ORIENTED_EDGE('',*,*,#3555,.T.);
#4617=ORIENTED_EDGE('',*,*,#3556,.F.);
#4618=ORIENTED_EDGE('',*,*,#3557,.F.);
#4619=ORIENTED_EDGE('',*,*,#3558,.F.);
#4620=ORIENTED_EDGE('',*,*,#3559,.F.);
#4621=ORIENTED_EDGE('',*,*,#3560,.F.);
#4622=ORIENTED_EDGE('',*,*,#3561,.F.);
#4623=ORIENTED_EDGE('',*,*,#3562,.F.);
#4624=ORIENTED_EDGE('',*,*,#3563,.F.);
#4625=ORIENTED_EDGE('',*,*,#3564,.F.);
#4626=ORIENTED_EDGE('',*,*,#3565,.F.);
#4627=ORIENTED_EDGE('',*,*,#3566,.F.);
#4628=ORIENTED_EDGE('',*,*,#3567,.F.);
#4629=ORIENTED_EDGE('',*,*,#3552,.T.);
#4630=ORIENTED_EDGE('',*,*,#3544,.T.);
#4631=ORIENTED_EDGE('',*,*,#3513,.T.);
#4632=ORIENTED_EDGE('',*,*,#3516,.T.);
#4633=ORIENTED_EDGE('',*,*,#3519,.T.);
#4634=ORIENTED_EDGE('',*,*,#3568,.F.);
#4635=ORIENTED_EDGE('',*,*,#3569,.F.);
#4636=ORIENTED_EDGE('',*,*,#3555,.F.);
#4637=ORIENTED_EDGE('',*,*,#3548,.T.);
#4638=ORIENTED_EDGE('',*,*,#3570,.F.);
#4639=ORIENTED_EDGE('',*,*,#3553,.T.);
#4640=ORIENTED_EDGE('',*,*,#3567,.T.);
#4641=ORIENTED_EDGE('',*,*,#3571,.T.);
#4642=ORIENTED_EDGE('',*,*,#3572,.F.);
#4643=ORIENTED_EDGE('',*,*,#3569,.T.);
#4644=ORIENTED_EDGE('',*,*,#3573,.F.);
#4645=ORIENTED_EDGE('',*,*,#3574,.T.);
#4646=ORIENTED_EDGE('',*,*,#3556,.T.);
#4647=ORIENTED_EDGE('',*,*,#3551,.T.);
#4648=ORIENTED_EDGE('',*,*,#3554,.T.);
#4649=ORIENTED_EDGE('',*,*,#3572,.T.);
#4650=ORIENTED_EDGE('',*,*,#3575,.T.);
#4651=ORIENTED_EDGE('',*,*,#3576,.T.);
#4652=ORIENTED_EDGE('',*,*,#3577,.T.);
#4653=ORIENTED_EDGE('',*,*,#3578,.T.);
#4654=ORIENTED_EDGE('',*,*,#3579,.T.);
#4655=ORIENTED_EDGE('',*,*,#3580,.T.);
#4656=ORIENTED_EDGE('',*,*,#3581,.T.);
#4657=ORIENTED_EDGE('',*,*,#3582,.T.);
#4658=ORIENTED_EDGE('',*,*,#3583,.T.);
#4659=ORIENTED_EDGE('',*,*,#3584,.T.);
#4660=ORIENTED_EDGE('',*,*,#3573,.T.);
#4661=ORIENTED_EDGE('',*,*,#3570,.T.);
#4662=ORIENTED_EDGE('',*,*,#3547,.T.);
#4663=ORIENTED_EDGE('',*,*,#3511,.T.);
#4664=ORIENTED_EDGE('',*,*,#3514,.T.);
#4665=ORIENTED_EDGE('',*,*,#3517,.T.);
#4666=ORIENTED_EDGE('',*,*,#3585,.F.);
#4667=ORIENTED_EDGE('',*,*,#3568,.T.);
#4668=ORIENTED_EDGE('',*,*,#3586,.T.);
#4669=ORIENTED_EDGE('',*,*,#3587,.T.);
#4670=ORIENTED_EDGE('',*,*,#3586,.F.);
#4671=ORIENTED_EDGE('',*,*,#3588,.F.);
#4672=ORIENTED_EDGE('',*,*,#3589,.F.);
#4673=ORIENTED_EDGE('',*,*,#3590,.T.);
#4674=ORIENTED_EDGE('',*,*,#3587,.F.);
#4675=ORIENTED_EDGE('',*,*,#3590,.F.);
#4676=ORIENTED_EDGE('',*,*,#3585,.T.);
#4677=ORIENTED_EDGE('',*,*,#3591,.T.);
#4678=ORIENTED_EDGE('',*,*,#3588,.T.);
#4679=ORIENTED_EDGE('',*,*,#3589,.T.);
#4680=ORIENTED_EDGE('',*,*,#3591,.F.);
#4681=ORIENTED_EDGE('',*,*,#3592,.F.);
#4682=ORIENTED_EDGE('',*,*,#3582,.F.);
#4683=ORIENTED_EDGE('',*,*,#3593,.F.);
#4684=ORIENTED_EDGE('',*,*,#3559,.T.);
#4685=ORIENTED_EDGE('',*,*,#3594,.F.);
#4686=ORIENTED_EDGE('',*,*,#3565,.T.);
#4687=ORIENTED_EDGE('',*,*,#3595,.F.);
#4688=ORIENTED_EDGE('',*,*,#3576,.F.);
#4689=ORIENTED_EDGE('',*,*,#3595,.T.);
#4690=ORIENTED_EDGE('',*,*,#3564,.T.);
#4691=ORIENTED_EDGE('',*,*,#3596,.T.);
#4692=ORIENTED_EDGE('',*,*,#3577,.F.);
#4693=ORIENTED_EDGE('',*,*,#3593,.T.);
#4694=ORIENTED_EDGE('',*,*,#3581,.F.);
#4695=ORIENTED_EDGE('',*,*,#3597,.F.);
#4696=ORIENTED_EDGE('',*,*,#3560,.T.);
#4697=ORIENTED_EDGE('',*,*,#3594,.T.);
#4698=ORIENTED_EDGE('',*,*,#3575,.F.);
#4699=ORIENTED_EDGE('',*,*,#3571,.F.);
#4700=ORIENTED_EDGE('',*,*,#3566,.T.);
#4701=ORIENTED_EDGE('',*,*,#3574,.F.);
#4702=ORIENTED_EDGE('',*,*,#3584,.F.);
#4703=ORIENTED_EDGE('',*,*,#3598,.F.);
#4704=ORIENTED_EDGE('',*,*,#3557,.T.);
#4705=ORIENTED_EDGE('',*,*,#3592,.T.);
#4706=ORIENTED_EDGE('',*,*,#3558,.T.);
#4707=ORIENTED_EDGE('',*,*,#3598,.T.);
#4708=ORIENTED_EDGE('',*,*,#3583,.F.);
#4709=ORIENTED_EDGE('',*,*,#3561,.T.);
#4710=ORIENTED_EDGE('',*,*,#3597,.T.);
#4711=ORIENTED_EDGE('',*,*,#3580,.F.);
#4712=ORIENTED_EDGE('',*,*,#3599,.F.);
#4713=ORIENTED_EDGE('',*,*,#3562,.T.);
#4714=ORIENTED_EDGE('',*,*,#3599,.T.);
#4715=ORIENTED_EDGE('',*,*,#3579,.F.);
#4716=ORIENTED_EDGE('',*,*,#3600,.F.);
#4717=ORIENTED_EDGE('',*,*,#3563,.T.);
#4718=ORIENTED_EDGE('',*,*,#3600,.T.);
#4719=ORIENTED_EDGE('',*,*,#3578,.F.);
#4720=ORIENTED_EDGE('',*,*,#3596,.F.);
#4721=ORIENTED_EDGE('',*,*,#3601,.F.);
#4722=ORIENTED_EDGE('',*,*,#3602,.T.);
#4723=ORIENTED_EDGE('',*,*,#3603,.F.);
#4724=ORIENTED_EDGE('',*,*,#3602,.F.);
#4725=ORIENTED_EDGE('',*,*,#3604,.F.);
#4726=ORIENTED_EDGE('',*,*,#3605,.T.);
#4727=ORIENTED_EDGE('',*,*,#3606,.F.);
#4728=ORIENTED_EDGE('',*,*,#3605,.F.);
#4729=ORIENTED_EDGE('',*,*,#3607,.F.);
#4730=ORIENTED_EDGE('',*,*,#3608,.T.);
#4731=ORIENTED_EDGE('',*,*,#3609,.F.);
#4732=ORIENTED_EDGE('',*,*,#3608,.F.);
#4733=ORIENTED_EDGE('',*,*,#3610,.F.);
#4734=ORIENTED_EDGE('',*,*,#3611,.F.);
#4735=ORIENTED_EDGE('',*,*,#3612,.T.);
#4736=ORIENTED_EDGE('',*,*,#3613,.F.);
#4737=ORIENTED_EDGE('',*,*,#3614,.F.);
#4738=ORIENTED_EDGE('',*,*,#3611,.T.);
#4739=ORIENTED_EDGE('',*,*,#3615,.F.);
#4740=ORIENTED_EDGE('',*,*,#3616,.F.);
#4741=ORIENTED_EDGE('',*,*,#3617,.F.);
#4742=ORIENTED_EDGE('',*,*,#3613,.T.);
#4743=ORIENTED_EDGE('',*,*,#3615,.T.);
#4744=ORIENTED_EDGE('',*,*,#3610,.T.);
#4745=ORIENTED_EDGE('',*,*,#3618,.T.);
#4746=ORIENTED_EDGE('',*,*,#3619,.F.);
#4747=ORIENTED_EDGE('',*,*,#3620,.T.);
#4748=ORIENTED_EDGE('',*,*,#3621,.T.);
#4749=ORIENTED_EDGE('',*,*,#3616,.T.);
#4750=ORIENTED_EDGE('',*,*,#3622,.T.);
#4751=ORIENTED_EDGE('',*,*,#3623,.F.);
#4752=ORIENTED_EDGE('',*,*,#3618,.F.);
#4753=ORIENTED_EDGE('',*,*,#3612,.F.);
#4754=ORIENTED_EDGE('',*,*,#3624,.F.);
#4755=ORIENTED_EDGE('',*,*,#3625,.T.);
#4756=ORIENTED_EDGE('',*,*,#3617,.T.);
#4757=ORIENTED_EDGE('',*,*,#3622,.F.);
#4758=ORIENTED_EDGE('',*,*,#3626,.F.);
#4759=ORIENTED_EDGE('',*,*,#3627,.T.);
#4760=ORIENTED_EDGE('',*,*,#3626,.T.);
#4761=ORIENTED_EDGE('',*,*,#3621,.F.);
#4762=ORIENTED_EDGE('',*,*,#3628,.F.);
#4763=ORIENTED_EDGE('',*,*,#3629,.T.);
#4764=ORIENTED_EDGE('',*,*,#3630,.T.);
#4765=ORIENTED_EDGE('',*,*,#3631,.T.);
#4766=ORIENTED_EDGE('',*,*,#3624,.T.);
#4767=ORIENTED_EDGE('',*,*,#3614,.T.);
#4768=ORIENTED_EDGE('',*,*,#3625,.F.);
#4769=ORIENTED_EDGE('',*,*,#3627,.F.);
#4770=ORIENTED_EDGE('',*,*,#3632,.T.);
#4771=ORIENTED_EDGE('',*,*,#3629,.F.);
#4772=ORIENTED_EDGE('',*,*,#3633,.T.);
#4773=ORIENTED_EDGE('',*,*,#3634,.F.);
#4774=ORIENTED_EDGE('',*,*,#3635,.F.);
#4775=ORIENTED_EDGE('',*,*,#3636,.F.);
#4776=ORIENTED_EDGE('',*,*,#3637,.F.);
#4777=ORIENTED_EDGE('',*,*,#3638,.F.);
#4778=ORIENTED_EDGE('',*,*,#3639,.F.);
#4779=ORIENTED_EDGE('',*,*,#3630,.F.);
#4780=ORIENTED_EDGE('',*,*,#3635,.T.);
#4781=ORIENTED_EDGE('',*,*,#3634,.T.);
#4782=ORIENTED_EDGE('',*,*,#3640,.T.);
#4783=ORIENTED_EDGE('',*,*,#3641,.T.);
#4784=ORIENTED_EDGE('',*,*,#3642,.F.);
#4785=ORIENTED_EDGE('',*,*,#3643,.F.);
#4786=ORIENTED_EDGE('',*,*,#3644,.F.);
#4787=ORIENTED_EDGE('',*,*,#3645,.F.);
#4788=ORIENTED_EDGE('',*,*,#3646,.F.);
#4789=ORIENTED_EDGE('',*,*,#3647,.F.);
#4790=ORIENTED_EDGE('',*,*,#3648,.F.);
#4791=ORIENTED_EDGE('',*,*,#3649,.F.);
#4792=ORIENTED_EDGE('',*,*,#3650,.F.);
#4793=ORIENTED_EDGE('',*,*,#3651,.F.);
#4794=ORIENTED_EDGE('',*,*,#3652,.F.);
#4795=ORIENTED_EDGE('',*,*,#3653,.F.);
#4796=ORIENTED_EDGE('',*,*,#3636,.T.);
#4797=ORIENTED_EDGE('',*,*,#3603,.T.);
#4798=ORIENTED_EDGE('',*,*,#3606,.T.);
#4799=ORIENTED_EDGE('',*,*,#3609,.T.);
#4800=ORIENTED_EDGE('',*,*,#3654,.F.);
#4801=ORIENTED_EDGE('',*,*,#3655,.T.);
#4802=ORIENTED_EDGE('',*,*,#3656,.F.);
#4803=ORIENTED_EDGE('',*,*,#3657,.F.);
#4804=ORIENTED_EDGE('',*,*,#3640,.F.);
#4805=ORIENTED_EDGE('',*,*,#3633,.F.);
#4806=ORIENTED_EDGE('',*,*,#3632,.F.);
#4807=ORIENTED_EDGE('',*,*,#3628,.T.);
#4808=ORIENTED_EDGE('',*,*,#3620,.F.);
#4809=ORIENTED_EDGE('',*,*,#3623,.T.);
#4810=ORIENTED_EDGE('',*,*,#3631,.F.);
#4811=ORIENTED_EDGE('',*,*,#3639,.T.);
#4812=ORIENTED_EDGE('',*,*,#3658,.F.);
#4813=ORIENTED_EDGE('',*,*,#3655,.F.);
#4814=ORIENTED_EDGE('',*,*,#3619,.T.);
#4815=ORIENTED_EDGE('',*,*,#3659,.F.);
#4816=ORIENTED_EDGE('',*,*,#3641,.F.);
#4817=ORIENTED_EDGE('',*,*,#3657,.T.);
#4818=ORIENTED_EDGE('',*,*,#3660,.F.);
#4819=ORIENTED_EDGE('',*,*,#3637,.T.);
#4820=ORIENTED_EDGE('',*,*,#3653,.T.);
#4821=ORIENTED_EDGE('',*,*,#3661,.T.);
#4822=ORIENTED_EDGE('',*,*,#3662,.F.);
#4823=ORIENTED_EDGE('',*,*,#3659,.T.);
#4824=ORIENTED_EDGE('',*,*,#3663,.F.);
#4825=ORIENTED_EDGE('',*,*,#3664,.T.);
#4826=ORIENTED_EDGE('',*,*,#3642,.T.);
#4827=ORIENTED_EDGE('',*,*,#3638,.T.);
#4828=ORIENTED_EDGE('',*,*,#3662,.T.);
#4829=ORIENTED_EDGE('',*,*,#3665,.T.);
#4830=ORIENTED_EDGE('',*,*,#3666,.T.);
#4831=ORIENTED_EDGE('',*,*,#3667,.T.);
#4832=ORIENTED_EDGE('',*,*,#3668,.T.);
#4833=ORIENTED_EDGE('',*,*,#3669,.T.);
#4834=ORIENTED_EDGE('',*,*,#3670,.T.);
#4835=ORIENTED_EDGE('',*,*,#3671,.T.);
#4836=ORIENTED_EDGE('',*,*,#3672,.T.);
#4837=ORIENTED_EDGE('',*,*,#3673,.T.);
#4838=ORIENTED_EDGE('',*,*,#3674,.T.);
#4839=ORIENTED_EDGE('',*,*,#3663,.T.);
#4840=ORIENTED_EDGE('',*,*,#3660,.T.);
#4841=ORIENTED_EDGE('',*,*,#3656,.T.);
#4842=ORIENTED_EDGE('',*,*,#3658,.T.);
#4843=ORIENTED_EDGE('',*,*,#3601,.T.);
#4844=ORIENTED_EDGE('',*,*,#3604,.T.);
#4845=ORIENTED_EDGE('',*,*,#3607,.T.);
#4846=ORIENTED_EDGE('',*,*,#3675,.F.);
#4847=ORIENTED_EDGE('',*,*,#3654,.T.);
#4848=ORIENTED_EDGE('',*,*,#3676,.T.);
#4849=ORIENTED_EDGE('',*,*,#3677,.T.);
#4850=ORIENTED_EDGE('',*,*,#3676,.F.);
#4851=ORIENTED_EDGE('',*,*,#3678,.F.);
#4852=ORIENTED_EDGE('',*,*,#3679,.F.);
#4853=ORIENTED_EDGE('',*,*,#3680,.T.);
#4854=ORIENTED_EDGE('',*,*,#3677,.F.);
#4855=ORIENTED_EDGE('',*,*,#3680,.F.);
#4856=ORIENTED_EDGE('',*,*,#3675,.T.);
#4857=ORIENTED_EDGE('',*,*,#3681,.T.);
#4858=ORIENTED_EDGE('',*,*,#3678,.T.);
#4859=ORIENTED_EDGE('',*,*,#3679,.T.);
#4860=ORIENTED_EDGE('',*,*,#3681,.F.);
#4861=ORIENTED_EDGE('',*,*,#3682,.F.);
#4862=ORIENTED_EDGE('',*,*,#3672,.F.);
#4863=ORIENTED_EDGE('',*,*,#3683,.F.);
#4864=ORIENTED_EDGE('',*,*,#3645,.T.);
#4865=ORIENTED_EDGE('',*,*,#3684,.F.);
#4866=ORIENTED_EDGE('',*,*,#3651,.T.);
#4867=ORIENTED_EDGE('',*,*,#3685,.F.);
#4868=ORIENTED_EDGE('',*,*,#3666,.F.);
#4869=ORIENTED_EDGE('',*,*,#3685,.T.);
#4870=ORIENTED_EDGE('',*,*,#3650,.T.);
#4871=ORIENTED_EDGE('',*,*,#3686,.T.);
#4872=ORIENTED_EDGE('',*,*,#3667,.F.);
#4873=ORIENTED_EDGE('',*,*,#3683,.T.);
#4874=ORIENTED_EDGE('',*,*,#3671,.F.);
#4875=ORIENTED_EDGE('',*,*,#3687,.F.);
#4876=ORIENTED_EDGE('',*,*,#3646,.T.);
#4877=ORIENTED_EDGE('',*,*,#3684,.T.);
#4878=ORIENTED_EDGE('',*,*,#3665,.F.);
#4879=ORIENTED_EDGE('',*,*,#3661,.F.);
#4880=ORIENTED_EDGE('',*,*,#3652,.T.);
#4881=ORIENTED_EDGE('',*,*,#3664,.F.);
#4882=ORIENTED_EDGE('',*,*,#3674,.F.);
#4883=ORIENTED_EDGE('',*,*,#3688,.F.);
#4884=ORIENTED_EDGE('',*,*,#3643,.T.);
#4885=ORIENTED_EDGE('',*,*,#3682,.T.);
#4886=ORIENTED_EDGE('',*,*,#3644,.T.);
#4887=ORIENTED_EDGE('',*,*,#3688,.T.);
#4888=ORIENTED_EDGE('',*,*,#3673,.F.);
#4889=ORIENTED_EDGE('',*,*,#3647,.T.);
#4890=ORIENTED_EDGE('',*,*,#3687,.T.);
#4891=ORIENTED_EDGE('',*,*,#3670,.F.);
#4892=ORIENTED_EDGE('',*,*,#3689,.F.);
#4893=ORIENTED_EDGE('',*,*,#3648,.T.);
#4894=ORIENTED_EDGE('',*,*,#3689,.T.);
#4895=ORIENTED_EDGE('',*,*,#3669,.F.);
#4896=ORIENTED_EDGE('',*,*,#3690,.F.);
#4897=ORIENTED_EDGE('',*,*,#3649,.T.);
#4898=ORIENTED_EDGE('',*,*,#3690,.T.);
#4899=ORIENTED_EDGE('',*,*,#3668,.F.);
#4900=ORIENTED_EDGE('',*,*,#3686,.F.);
#4901=ORIENTED_EDGE('',*,*,#3691,.T.);
#4902=ORIENTED_EDGE('',*,*,#3692,.T.);
#4903=ORIENTED_EDGE('',*,*,#3693,.F.);
#4904=ORIENTED_EDGE('',*,*,#3692,.F.);
#4905=ORIENTED_EDGE('',*,*,#3694,.F.);
#4906=ORIENTED_EDGE('',*,*,#3691,.F.);
#4907=ORIENTED_EDGE('',*,*,#3695,.F.);
#4908=ORIENTED_EDGE('',*,*,#3693,.T.);
#4909=ORIENTED_EDGE('',*,*,#3696,.F.);
#4910=ORIENTED_EDGE('',*,*,#3697,.T.);
#4911=ORIENTED_EDGE('',*,*,#3695,.T.);
#4912=ORIENTED_EDGE('',*,*,#3697,.F.);
#4913=ORIENTED_EDGE('',*,*,#3698,.T.);
#4914=ORIENTED_EDGE('',*,*,#3699,.F.);
#4915=ORIENTED_EDGE('',*,*,#3698,.F.);
#4916=ORIENTED_EDGE('',*,*,#3700,.T.);
#4917=ORIENTED_EDGE('',*,*,#3701,.T.);
#4918=ORIENTED_EDGE('',*,*,#3700,.F.);
#4919=ORIENTED_EDGE('',*,*,#3701,.F.);
#4920=ORIENTED_EDGE('',*,*,#3694,.T.);
#4921=ORIENTED_EDGE('',*,*,#3702,.T.);
#4922=ORIENTED_EDGE('',*,*,#3699,.T.);
#4923=ORIENTED_EDGE('',*,*,#3702,.F.);
#4924=ORIENTED_EDGE('',*,*,#3696,.T.);
#4925=ORIENTED_EDGE('',*,*,#3703,.F.);
#4926=ORIENTED_EDGE('',*,*,#3704,.F.);
#4927=ORIENTED_EDGE('',*,*,#3705,.F.);
#4928=ORIENTED_EDGE('',*,*,#3706,.F.);
#4929=ORIENTED_EDGE('',*,*,#3707,.F.);
#4930=ORIENTED_EDGE('',*,*,#3708,.F.);
#4931=ORIENTED_EDGE('',*,*,#3709,.F.);
#4932=ORIENTED_EDGE('',*,*,#3710,.F.);
#4933=ORIENTED_EDGE('',*,*,#3710,.T.);
#4934=ORIENTED_EDGE('',*,*,#3711,.F.);
#4935=ORIENTED_EDGE('',*,*,#3704,.T.);
#4936=ORIENTED_EDGE('',*,*,#3712,.F.);
#4937=ORIENTED_EDGE('',*,*,#3707,.T.);
#4938=ORIENTED_EDGE('',*,*,#3712,.T.);
#4939=ORIENTED_EDGE('',*,*,#3703,.T.);
#4940=ORIENTED_EDGE('',*,*,#3713,.F.);
#4941=ORIENTED_EDGE('',*,*,#3709,.T.);
#4942=ORIENTED_EDGE('',*,*,#3714,.F.);
#4943=ORIENTED_EDGE('',*,*,#3705,.T.);
#4944=ORIENTED_EDGE('',*,*,#3711,.T.);
#4945=ORIENTED_EDGE('',*,*,#3708,.T.);
#4946=ORIENTED_EDGE('',*,*,#3713,.T.);
#4947=ORIENTED_EDGE('',*,*,#3706,.T.);
#4948=ORIENTED_EDGE('',*,*,#3714,.T.);
#4949=ORIENTED_EDGE('',*,*,#3715,.F.);
#4950=ORIENTED_EDGE('',*,*,#3716,.T.);
#4951=ORIENTED_EDGE('',*,*,#3717,.F.);
#4952=ORIENTED_EDGE('',*,*,#3716,.F.);
#4953=ORIENTED_EDGE('',*,*,#3718,.F.);
#4954=ORIENTED_EDGE('',*,*,#3719,.T.);
#4955=ORIENTED_EDGE('',*,*,#3720,.F.);
#4956=ORIENTED_EDGE('',*,*,#3719,.F.);
#4957=ORIENTED_EDGE('',*,*,#3721,.F.);
#4958=ORIENTED_EDGE('',*,*,#3722,.T.);
#4959=ORIENTED_EDGE('',*,*,#3723,.F.);
#4960=ORIENTED_EDGE('',*,*,#3722,.F.);
#4961=ORIENTED_EDGE('',*,*,#3724,.F.);
#4962=ORIENTED_EDGE('',*,*,#3725,.T.);
#4963=ORIENTED_EDGE('',*,*,#3726,.F.);
#4964=ORIENTED_EDGE('',*,*,#3725,.F.);
#4965=ORIENTED_EDGE('',*,*,#3727,.F.);
#4966=ORIENTED_EDGE('',*,*,#3728,.T.);
#4967=ORIENTED_EDGE('',*,*,#3729,.T.);
#4968=ORIENTED_EDGE('',*,*,#3728,.F.);
#4969=ORIENTED_EDGE('',*,*,#3729,.F.);
#4970=ORIENTED_EDGE('',*,*,#3730,.F.);
#4971=ORIENTED_EDGE('',*,*,#3731,.F.);
#4972=ORIENTED_EDGE('',*,*,#3732,.T.);
#4973=ORIENTED_EDGE('',*,*,#3733,.T.);
#4974=ORIENTED_EDGE('',*,*,#3732,.F.);
#4975=ORIENTED_EDGE('',*,*,#3733,.F.);
#4976=ORIENTED_EDGE('',*,*,#3734,.F.);
#4977=ORIENTED_EDGE('',*,*,#3730,.T.);
#4978=ORIENTED_EDGE('',*,*,#3735,.T.);
#4979=ORIENTED_EDGE('',*,*,#3736,.F.);
#4980=ORIENTED_EDGE('',*,*,#3735,.F.);
#4981=ORIENTED_EDGE('',*,*,#3734,.T.);
#4982=ORIENTED_EDGE('',*,*,#3737,.T.);
#4983=ORIENTED_EDGE('',*,*,#3738,.F.);
#4984=ORIENTED_EDGE('',*,*,#3737,.F.);
#4985=ORIENTED_EDGE('',*,*,#3739,.F.);
#4986=ORIENTED_EDGE('',*,*,#3740,.F.);
#4987=ORIENTED_EDGE('',*,*,#3741,.F.);
#4988=ORIENTED_EDGE('',*,*,#3742,.T.);
#4989=ORIENTED_EDGE('',*,*,#3743,.F.);
#4990=ORIENTED_EDGE('',*,*,#3744,.T.);
#4991=ORIENTED_EDGE('',*,*,#3745,.F.);
#4992=ORIENTED_EDGE('',*,*,#3746,.F.);
#4993=ORIENTED_EDGE('',*,*,#3747,.F.);
#4994=ORIENTED_EDGE('',*,*,#3748,.T.);
#4995=ORIENTED_EDGE('',*,*,#3749,.F.);
#4996=ORIENTED_EDGE('',*,*,#3750,.F.);
#4997=ORIENTED_EDGE('',*,*,#3751,.F.);
#4998=ORIENTED_EDGE('',*,*,#3752,.T.);
#4999=ORIENTED_EDGE('',*,*,#3753,.F.);
#5000=ORIENTED_EDGE('',*,*,#3754,.F.);
#5001=ORIENTED_EDGE('',*,*,#3755,.F.);
#5002=ORIENTED_EDGE('',*,*,#3756,.T.);
#5003=ORIENTED_EDGE('',*,*,#3757,.F.);
#5004=ORIENTED_EDGE('',*,*,#3758,.F.);
#5005=ORIENTED_EDGE('',*,*,#3759,.F.);
#5006=ORIENTED_EDGE('',*,*,#3760,.F.);
#5007=ORIENTED_EDGE('',*,*,#3761,.F.);
#5008=ORIENTED_EDGE('',*,*,#3762,.T.);
#5009=ORIENTED_EDGE('',*,*,#3763,.F.);
#5010=ORIENTED_EDGE('',*,*,#3764,.F.);
#5011=ORIENTED_EDGE('',*,*,#3765,.F.);
#5012=ORIENTED_EDGE('',*,*,#3766,.T.);
#5013=ORIENTED_EDGE('',*,*,#3767,.F.);
#5014=ORIENTED_EDGE('',*,*,#3736,.T.);
#5015=ORIENTED_EDGE('',*,*,#3768,.F.);
#5016=ORIENTED_EDGE('',*,*,#3738,.T.);
#5017=ORIENTED_EDGE('',*,*,#3769,.F.);
#5018=ORIENTED_EDGE('',*,*,#3742,.F.);
#5019=ORIENTED_EDGE('',*,*,#3770,.F.);
#5020=ORIENTED_EDGE('',*,*,#3756,.F.);
#5021=ORIENTED_EDGE('',*,*,#3771,.F.);
#5022=ORIENTED_EDGE('',*,*,#3762,.F.);
#5023=ORIENTED_EDGE('',*,*,#3772,.F.);
#5024=ORIENTED_EDGE('',*,*,#3744,.F.);
#5025=ORIENTED_EDGE('',*,*,#3773,.F.);
#5026=ORIENTED_EDGE('',*,*,#3766,.F.);
#5027=ORIENTED_EDGE('',*,*,#3774,.F.);
#5028=ORIENTED_EDGE('',*,*,#3748,.F.);
#5029=ORIENTED_EDGE('',*,*,#3775,.F.);
#5030=ORIENTED_EDGE('',*,*,#3776,.F.);
#5031=ORIENTED_EDGE('',*,*,#3777,.F.);
#5032=ORIENTED_EDGE('',*,*,#3752,.F.);
#5033=ORIENTED_EDGE('',*,*,#3778,.F.);
#5034=ORIENTED_EDGE('',*,*,#3779,.F.);
#5035=ORIENTED_EDGE('',*,*,#3780,.F.);
#5036=ORIENTED_EDGE('',*,*,#3776,.T.);
#5037=ORIENTED_EDGE('',*,*,#3781,.T.);
#5038=ORIENTED_EDGE('',*,*,#3782,.F.);
#5039=ORIENTED_EDGE('',*,*,#3783,.F.);
#5040=ORIENTED_EDGE('',*,*,#3784,.F.);
#5041=ORIENTED_EDGE('',*,*,#3785,.F.);
#5042=ORIENTED_EDGE('',*,*,#3786,.F.);
#5043=ORIENTED_EDGE('',*,*,#3753,.T.);
#5044=ORIENTED_EDGE('',*,*,#3777,.T.);
#5045=ORIENTED_EDGE('',*,*,#3780,.T.);
#5046=ORIENTED_EDGE('',*,*,#3787,.T.);
#5047=ORIENTED_EDGE('',*,*,#3788,.F.);
#5048=ORIENTED_EDGE('',*,*,#3789,.F.);
#5049=ORIENTED_EDGE('',*,*,#3790,.F.);
#5050=ORIENTED_EDGE('',*,*,#3791,.F.);
#5051=ORIENTED_EDGE('',*,*,#3792,.F.);
#5052=ORIENTED_EDGE('',*,*,#3793,.T.);
#5053=ORIENTED_EDGE('',*,*,#3749,.T.);
#5054=ORIENTED_EDGE('',*,*,#3774,.T.);
#5055=ORIENTED_EDGE('',*,*,#3765,.T.);
#5056=ORIENTED_EDGE('',*,*,#3794,.T.);
#5057=ORIENTED_EDGE('',*,*,#3795,.F.);
#5058=ORIENTED_EDGE('',*,*,#3796,.F.);
#5059=ORIENTED_EDGE('',*,*,#3797,.F.);
#5060=ORIENTED_EDGE('',*,*,#3798,.F.);
#5061=ORIENTED_EDGE('',*,*,#3799,.F.);
#5062=ORIENTED_EDGE('',*,*,#3800,.T.);
#5063=ORIENTED_EDGE('',*,*,#3745,.T.);
#5064=ORIENTED_EDGE('',*,*,#3772,.T.);
#5065=ORIENTED_EDGE('',*,*,#3761,.T.);
#5066=ORIENTED_EDGE('',*,*,#3801,.T.);
#5067=ORIENTED_EDGE('',*,*,#3802,.F.);
#5068=ORIENTED_EDGE('',*,*,#3803,.F.);
#5069=ORIENTED_EDGE('',*,*,#3804,.F.);
#5070=ORIENTED_EDGE('',*,*,#3805,.F.);
#5071=ORIENTED_EDGE('',*,*,#3806,.F.);
#5072=ORIENTED_EDGE('',*,*,#3807,.T.);
#5073=ORIENTED_EDGE('',*,*,#3739,.T.);
#5074=ORIENTED_EDGE('',*,*,#3769,.T.);
#5075=ORIENTED_EDGE('',*,*,#3755,.T.);
#5076=ORIENTED_EDGE('',*,*,#3808,.F.);
#5077=ORIENTED_EDGE('',*,*,#3809,.T.);
#5078=ORIENTED_EDGE('',*,*,#3810,.T.);
#5079=ORIENTED_EDGE('',*,*,#3811,.T.);
#5080=ORIENTED_EDGE('',*,*,#3812,.F.);
#5081=ORIENTED_EDGE('',*,*,#3754,.T.);
#5082=ORIENTED_EDGE('',*,*,#3793,.F.);
#5083=ORIENTED_EDGE('',*,*,#3813,.T.);
#5084=ORIENTED_EDGE('',*,*,#3781,.F.);
#5085=ORIENTED_EDGE('',*,*,#3814,.T.);
#5086=ORIENTED_EDGE('',*,*,#3787,.F.);
#5087=ORIENTED_EDGE('',*,*,#3779,.T.);
#5088=ORIENTED_EDGE('',*,*,#3815,.F.);
#5089=ORIENTED_EDGE('',*,*,#3816,.T.);
#5090=ORIENTED_EDGE('',*,*,#3794,.F.);
#5091=ORIENTED_EDGE('',*,*,#3764,.T.);
#5092=ORIENTED_EDGE('',*,*,#3817,.F.);
#5093=ORIENTED_EDGE('',*,*,#3818,.T.);
#5094=ORIENTED_EDGE('',*,*,#3801,.F.);
#5095=ORIENTED_EDGE('',*,*,#3760,.T.);
#5096=ORIENTED_EDGE('',*,*,#3819,.F.);
#5097=ORIENTED_EDGE('',*,*,#3820,.T.);
#5098=ORIENTED_EDGE('',*,*,#3821,.T.);
#5099=ORIENTED_EDGE('',*,*,#3808,.T.);
#5100=ORIENTED_EDGE('',*,*,#3758,.T.);
#5101=ORIENTED_EDGE('',*,*,#3822,.T.);
#5102=ORIENTED_EDGE('',*,*,#3823,.F.);
#5103=ORIENTED_EDGE('',*,*,#3824,.T.);
#5104=ORIENTED_EDGE('',*,*,#3825,.F.);
#5105=ORIENTED_EDGE('',*,*,#3826,.T.);
#5106=ORIENTED_EDGE('',*,*,#3827,.F.);
#5107=ORIENTED_EDGE('',*,*,#3828,.T.);
#5108=ORIENTED_EDGE('',*,*,#3829,.F.);
#5109=ORIENTED_EDGE('',*,*,#3830,.T.);
#5110=ORIENTED_EDGE('',*,*,#3740,.T.);
#5111=ORIENTED_EDGE('',*,*,#3812,.T.);
#5112=ORIENTED_EDGE('',*,*,#3831,.T.);
#5113=ORIENTED_EDGE('',*,*,#3832,.T.);
#5114=ORIENTED_EDGE('',*,*,#3833,.F.);
#5115=ORIENTED_EDGE('',*,*,#3746,.T.);
#5116=ORIENTED_EDGE('',*,*,#3807,.F.);
#5117=ORIENTED_EDGE('',*,*,#3834,.T.);
#5118=ORIENTED_EDGE('',*,*,#3835,.F.);
#5119=ORIENTED_EDGE('',*,*,#3750,.T.);
#5120=ORIENTED_EDGE('',*,*,#3800,.F.);
#5121=ORIENTED_EDGE('',*,*,#3836,.T.);
#5122=ORIENTED_EDGE('',*,*,#3837,.F.);
#5123=ORIENTED_EDGE('',*,*,#3838,.T.);
#5124=ORIENTED_EDGE('',*,*,#3839,.T.);
#5125=ORIENTED_EDGE('',*,*,#3840,.T.);
#5126=ORIENTED_EDGE('',*,*,#3841,.T.);
#5127=ORIENTED_EDGE('',*,*,#3842,.T.);
#5128=ORIENTED_EDGE('',*,*,#3843,.F.);
#5129=ORIENTED_EDGE('',*,*,#3844,.F.);
#5130=ORIENTED_EDGE('',*,*,#3845,.T.);
#5131=ORIENTED_EDGE('',*,*,#3768,.T.);
#5132=ORIENTED_EDGE('',*,*,#3845,.F.);
#5133=ORIENTED_EDGE('',*,*,#3846,.F.);
#5134=ORIENTED_EDGE('',*,*,#3847,.T.);
#5135=ORIENTED_EDGE('',*,*,#3767,.T.);
#5136=ORIENTED_EDGE('',*,*,#3847,.F.);
#5137=ORIENTED_EDGE('',*,*,#3848,.F.);
#5138=ORIENTED_EDGE('',*,*,#3843,.T.);
#5139=ORIENTED_EDGE('',*,*,#3849,.F.);
#5140=ORIENTED_EDGE('',*,*,#3850,.F.);
#5141=ORIENTED_EDGE('',*,*,#3851,.F.);
#5142=ORIENTED_EDGE('',*,*,#3852,.F.);
#5143=ORIENTED_EDGE('',*,*,#3782,.T.);
#5144=ORIENTED_EDGE('',*,*,#3813,.F.);
#5145=ORIENTED_EDGE('',*,*,#3792,.T.);
#5146=ORIENTED_EDGE('',*,*,#3853,.T.);
#5147=ORIENTED_EDGE('',*,*,#3848,.T.);
#5148=ORIENTED_EDGE('',*,*,#3854,.T.);
#5149=ORIENTED_EDGE('',*,*,#3855,.T.);
#5150=ORIENTED_EDGE('',*,*,#3838,.F.);
#5151=ORIENTED_EDGE('',*,*,#3783,.T.);
#5152=ORIENTED_EDGE('',*,*,#3853,.F.);
#5153=ORIENTED_EDGE('',*,*,#3791,.T.);
#5154=ORIENTED_EDGE('',*,*,#3856,.F.);
#5155=ORIENTED_EDGE('',*,*,#3852,.T.);
#5156=ORIENTED_EDGE('',*,*,#3857,.F.);
#5157=ORIENTED_EDGE('',*,*,#3858,.F.);
#5158=ORIENTED_EDGE('',*,*,#3854,.F.);
#5159=ORIENTED_EDGE('',*,*,#3784,.T.);
#5160=ORIENTED_EDGE('',*,*,#3856,.T.);
#5161=ORIENTED_EDGE('',*,*,#3790,.T.);
#5162=ORIENTED_EDGE('',*,*,#3859,.T.);
#5163=ORIENTED_EDGE('',*,*,#3717,.T.);
#5164=ORIENTED_EDGE('',*,*,#3726,.T.);
#5165=ORIENTED_EDGE('',*,*,#3844,.T.);
#5166=ORIENTED_EDGE('',*,*,#3851,.T.);
#5167=ORIENTED_EDGE('',*,*,#3860,.T.);
#5168=ORIENTED_EDGE('',*,*,#3861,.T.);
#5169=ORIENTED_EDGE('',*,*,#3857,.T.);
#5170=ORIENTED_EDGE('',*,*,#3785,.T.);
#5171=ORIENTED_EDGE('',*,*,#3859,.F.);
#5172=ORIENTED_EDGE('',*,*,#3789,.T.);
#5173=ORIENTED_EDGE('',*,*,#3862,.F.);
#5174=ORIENTED_EDGE('',*,*,#3786,.T.);
#5175=ORIENTED_EDGE('',*,*,#3862,.T.);
#5176=ORIENTED_EDGE('',*,*,#3788,.T.);
#5177=ORIENTED_EDGE('',*,*,#3814,.F.);
#5178=ORIENTED_EDGE('',*,*,#3849,.T.);
#5179=ORIENTED_EDGE('',*,*,#3842,.F.);
#5180=ORIENTED_EDGE('',*,*,#3863,.T.);
#5181=ORIENTED_EDGE('',*,*,#3864,.T.);
#5182=ORIENTED_EDGE('',*,*,#3751,.T.);
#5183=ORIENTED_EDGE('',*,*,#3837,.T.);
#5184=ORIENTED_EDGE('',*,*,#3865,.F.);
#5185=ORIENTED_EDGE('',*,*,#3866,.F.);
#5186=ORIENTED_EDGE('',*,*,#3867,.F.);
#5187=ORIENTED_EDGE('',*,*,#3868,.F.);
#5188=ORIENTED_EDGE('',*,*,#3869,.F.);
#5189=ORIENTED_EDGE('',*,*,#3815,.T.);
#5190=ORIENTED_EDGE('',*,*,#3778,.T.);
#5191=ORIENTED_EDGE('',*,*,#3775,.T.);
#5192=ORIENTED_EDGE('',*,*,#3865,.T.);
#5193=ORIENTED_EDGE('',*,*,#3836,.F.);
#5194=ORIENTED_EDGE('',*,*,#3799,.T.);
#5195=ORIENTED_EDGE('',*,*,#3870,.T.);
#5196=ORIENTED_EDGE('',*,*,#3866,.T.);
#5197=ORIENTED_EDGE('',*,*,#3870,.F.);
#5198=ORIENTED_EDGE('',*,*,#3798,.T.);
#5199=ORIENTED_EDGE('',*,*,#3871,.F.);
#5200=ORIENTED_EDGE('',*,*,#3867,.T.);
#5201=ORIENTED_EDGE('',*,*,#3871,.T.);
#5202=ORIENTED_EDGE('',*,*,#3797,.T.);
#5203=ORIENTED_EDGE('',*,*,#3872,.T.);
#5204=ORIENTED_EDGE('',*,*,#3868,.T.);
#5205=ORIENTED_EDGE('',*,*,#3872,.F.);
#5206=ORIENTED_EDGE('',*,*,#3796,.T.);
#5207=ORIENTED_EDGE('',*,*,#3873,.F.);
#5208=ORIENTED_EDGE('',*,*,#3869,.T.);
#5209=ORIENTED_EDGE('',*,*,#3873,.T.);
#5210=ORIENTED_EDGE('',*,*,#3795,.T.);
#5211=ORIENTED_EDGE('',*,*,#3816,.F.);
#5212=ORIENTED_EDGE('',*,*,#3747,.T.);
#5213=ORIENTED_EDGE('',*,*,#3835,.T.);
#5214=ORIENTED_EDGE('',*,*,#3874,.F.);
#5215=ORIENTED_EDGE('',*,*,#3875,.F.);
#5216=ORIENTED_EDGE('',*,*,#3876,.F.);
#5217=ORIENTED_EDGE('',*,*,#3877,.F.);
#5218=ORIENTED_EDGE('',*,*,#3878,.F.);
#5219=ORIENTED_EDGE('',*,*,#3817,.T.);
#5220=ORIENTED_EDGE('',*,*,#3763,.T.);
#5221=ORIENTED_EDGE('',*,*,#3773,.T.);
#5222=ORIENTED_EDGE('',*,*,#3874,.T.);
#5223=ORIENTED_EDGE('',*,*,#3834,.F.);
#5224=ORIENTED_EDGE('',*,*,#3806,.T.);
#5225=ORIENTED_EDGE('',*,*,#3879,.T.);
#5226=ORIENTED_EDGE('',*,*,#3875,.T.);
#5227=ORIENTED_EDGE('',*,*,#3879,.F.);
#5228=ORIENTED_EDGE('',*,*,#3805,.T.);
#5229=ORIENTED_EDGE('',*,*,#3880,.F.);
#5230=ORIENTED_EDGE('',*,*,#3876,.T.);
#5231=ORIENTED_EDGE('',*,*,#3880,.T.);
#5232=ORIENTED_EDGE('',*,*,#3804,.T.);
#5233=ORIENTED_EDGE('',*,*,#3881,.T.);
#5234=ORIENTED_EDGE('',*,*,#3720,.T.);
#5235=ORIENTED_EDGE('',*,*,#3723,.T.);
#5236=ORIENTED_EDGE('',*,*,#3846,.T.);
#5237=ORIENTED_EDGE('',*,*,#3877,.T.);
#5238=ORIENTED_EDGE('',*,*,#3881,.F.);
#5239=ORIENTED_EDGE('',*,*,#3803,.T.);
#5240=ORIENTED_EDGE('',*,*,#3882,.F.);
#5241=ORIENTED_EDGE('',*,*,#3878,.T.);
#5242=ORIENTED_EDGE('',*,*,#3882,.T.);
#5243=ORIENTED_EDGE('',*,*,#3802,.T.);
#5244=ORIENTED_EDGE('',*,*,#3818,.F.);
#5245=ORIENTED_EDGE('',*,*,#3743,.T.);
#5246=ORIENTED_EDGE('',*,*,#3833,.T.);
#5247=ORIENTED_EDGE('',*,*,#3883,.F.);
#5248=ORIENTED_EDGE('',*,*,#3884,.F.);
#5249=ORIENTED_EDGE('',*,*,#3885,.F.);
#5250=ORIENTED_EDGE('',*,*,#3886,.F.);
#5251=ORIENTED_EDGE('',*,*,#3887,.F.);
#5252=ORIENTED_EDGE('',*,*,#3819,.T.);
#5253=ORIENTED_EDGE('',*,*,#3759,.T.);
#5254=ORIENTED_EDGE('',*,*,#3771,.T.);
#5255=ORIENTED_EDGE('',*,*,#3883,.T.);
#5256=ORIENTED_EDGE('',*,*,#3832,.F.);
#5257=ORIENTED_EDGE('',*,*,#3888,.T.);
#5258=ORIENTED_EDGE('',*,*,#3889,.T.);
#5259=ORIENTED_EDGE('',*,*,#3884,.T.);
#5260=ORIENTED_EDGE('',*,*,#3889,.F.);
#5261=ORIENTED_EDGE('',*,*,#3890,.F.);
#5262=ORIENTED_EDGE('',*,*,#3891,.F.);
#5263=ORIENTED_EDGE('',*,*,#3885,.T.);
#5264=ORIENTED_EDGE('',*,*,#3891,.T.);
#5265=ORIENTED_EDGE('',*,*,#3892,.T.);
#5266=ORIENTED_EDGE('',*,*,#3893,.T.);
#5267=ORIENTED_EDGE('',*,*,#3887,.T.);
#5268=ORIENTED_EDGE('',*,*,#3894,.T.);
#5269=ORIENTED_EDGE('',*,*,#3895,.T.);
#5270=ORIENTED_EDGE('',*,*,#3820,.F.);
#5271=ORIENTED_EDGE('',*,*,#3886,.T.);
#5272=ORIENTED_EDGE('',*,*,#3893,.F.);
#5273=ORIENTED_EDGE('',*,*,#3896,.F.);
#5274=ORIENTED_EDGE('',*,*,#3894,.F.);
#5275=ORIENTED_EDGE('',*,*,#3897,.T.);
#5276=ORIENTED_EDGE('',*,*,#3898,.T.);
#5277=ORIENTED_EDGE('',*,*,#3896,.T.);
#5278=ORIENTED_EDGE('',*,*,#3899,.T.);
#5279=ORIENTED_EDGE('',*,*,#3900,.T.);
#5280=ORIENTED_EDGE('',*,*,#3901,.T.);
#5281=ORIENTED_EDGE('',*,*,#3890,.T.);
#5282=ORIENTED_EDGE('',*,*,#3902,.T.);
#5283=ORIENTED_EDGE('',*,*,#3903,.T.);
#5284=ORIENTED_EDGE('',*,*,#3897,.F.);
#5285=ORIENTED_EDGE('',*,*,#3892,.F.);
#5286=ORIENTED_EDGE('',*,*,#3903,.F.);
#5287=ORIENTED_EDGE('',*,*,#3810,.F.);
#5288=ORIENTED_EDGE('',*,*,#3831,.F.);
#5289=ORIENTED_EDGE('',*,*,#3811,.F.);
#5290=ORIENTED_EDGE('',*,*,#3902,.F.);
#5291=ORIENTED_EDGE('',*,*,#3888,.F.);
#5292=ORIENTED_EDGE('',*,*,#3904,.T.);
#5293=ORIENTED_EDGE('',*,*,#3858,.T.);
#5294=ORIENTED_EDGE('',*,*,#3905,.T.);
#5295=ORIENTED_EDGE('',*,*,#3905,.F.);
#5296=ORIENTED_EDGE('',*,*,#3861,.F.);
#5297=ORIENTED_EDGE('',*,*,#3901,.F.);
#5298=ORIENTED_EDGE('',*,*,#3906,.F.);
#5299=ORIENTED_EDGE('',*,*,#3839,.F.);
#5300=ORIENTED_EDGE('',*,*,#3855,.F.);
#5301=ORIENTED_EDGE('',*,*,#3904,.F.);
#5302=ORIENTED_EDGE('',*,*,#3907,.F.);
#5303=ORIENTED_EDGE('',*,*,#3841,.F.);
#5304=ORIENTED_EDGE('',*,*,#3908,.F.);
#5305=ORIENTED_EDGE('',*,*,#3900,.F.);
#5306=ORIENTED_EDGE('',*,*,#3863,.F.);
#5307=ORIENTED_EDGE('',*,*,#3850,.T.);
#5308=ORIENTED_EDGE('',*,*,#3864,.F.);
#5309=ORIENTED_EDGE('',*,*,#3899,.F.);
#5310=ORIENTED_EDGE('',*,*,#3860,.F.);
#5311=ORIENTED_EDGE('',*,*,#3821,.F.);
#5312=ORIENTED_EDGE('',*,*,#3895,.F.);
#5313=ORIENTED_EDGE('',*,*,#3898,.F.);
#5314=ORIENTED_EDGE('',*,*,#3809,.F.);
#5315=ORIENTED_EDGE('',*,*,#3907,.T.);
#5316=ORIENTED_EDGE('',*,*,#3906,.T.);
#5317=ORIENTED_EDGE('',*,*,#3908,.T.);
#5318=ORIENTED_EDGE('',*,*,#3840,.F.);
#5319=ORIENTED_EDGE('',*,*,#3909,.F.);
#5320=ORIENTED_EDGE('',*,*,#3910,.F.);
#5321=ORIENTED_EDGE('',*,*,#3911,.F.);
#5322=ORIENTED_EDGE('',*,*,#3912,.F.);
#5323=ORIENTED_EDGE('',*,*,#3913,.F.);
#5324=ORIENTED_EDGE('',*,*,#3914,.F.);
#5325=ORIENTED_EDGE('',*,*,#3915,.F.);
#5326=ORIENTED_EDGE('',*,*,#3916,.F.);
#5327=ORIENTED_EDGE('',*,*,#3917,.F.);
#5328=ORIENTED_EDGE('',*,*,#3909,.T.);
#5329=ORIENTED_EDGE('',*,*,#3918,.T.);
#5330=ORIENTED_EDGE('',*,*,#3916,.T.);
#5331=ORIENTED_EDGE('',*,*,#3919,.T.);
#5332=ORIENTED_EDGE('',*,*,#3829,.T.);
#5333=ORIENTED_EDGE('',*,*,#3920,.T.);
#5334=ORIENTED_EDGE('',*,*,#3917,.T.);
#5335=ORIENTED_EDGE('',*,*,#3921,.T.);
#5336=ORIENTED_EDGE('',*,*,#3922,.F.);
#5337=ORIENTED_EDGE('',*,*,#3923,.F.);
#5338=ORIENTED_EDGE('',*,*,#3924,.F.);
#5339=ORIENTED_EDGE('',*,*,#3923,.T.);
#5340=ORIENTED_EDGE('',*,*,#3925,.T.);
#5341=ORIENTED_EDGE('',*,*,#3913,.T.);
#5342=ORIENTED_EDGE('',*,*,#3926,.T.);
#5343=ORIENTED_EDGE('',*,*,#3915,.T.);
#5344=ORIENTED_EDGE('',*,*,#3927,.T.);
#5345=ORIENTED_EDGE('',*,*,#3924,.T.);
#5346=ORIENTED_EDGE('',*,*,#3928,.T.);
#5347=ORIENTED_EDGE('',*,*,#3827,.T.);
#5348=ORIENTED_EDGE('',*,*,#3929,.T.);
#5349=ORIENTED_EDGE('',*,*,#3922,.T.);
#5350=ORIENTED_EDGE('',*,*,#3930,.T.);
#5351=ORIENTED_EDGE('',*,*,#3825,.T.);
#5352=ORIENTED_EDGE('',*,*,#3931,.T.);
#5353=ORIENTED_EDGE('',*,*,#3914,.T.);
#5354=ORIENTED_EDGE('',*,*,#3932,.T.);
#5355=ORIENTED_EDGE('',*,*,#3912,.T.);
#5356=ORIENTED_EDGE('',*,*,#3933,.T.);
#5357=ORIENTED_EDGE('',*,*,#3910,.T.);
#5358=ORIENTED_EDGE('',*,*,#3934,.T.);
#5359=ORIENTED_EDGE('',*,*,#3823,.T.);
#5360=ORIENTED_EDGE('',*,*,#3935,.T.);
#5361=ORIENTED_EDGE('',*,*,#3911,.T.);
#5362=ORIENTED_EDGE('',*,*,#3936,.T.);
#5363=ORIENTED_EDGE('',*,*,#3930,.F.);
#5364=ORIENTED_EDGE('',*,*,#3927,.F.);
#5365=ORIENTED_EDGE('',*,*,#3920,.F.);
#5366=ORIENTED_EDGE('',*,*,#3828,.F.);
#5367=ORIENTED_EDGE('',*,*,#3741,.T.);
#5368=ORIENTED_EDGE('',*,*,#3830,.F.);
#5369=ORIENTED_EDGE('',*,*,#3921,.F.);
#5370=ORIENTED_EDGE('',*,*,#3918,.F.);
#5371=ORIENTED_EDGE('',*,*,#3935,.F.);
#5372=ORIENTED_EDGE('',*,*,#3822,.F.);
#5373=ORIENTED_EDGE('',*,*,#3757,.T.);
#5374=ORIENTED_EDGE('',*,*,#3770,.T.);
#5375=ORIENTED_EDGE('',*,*,#3926,.F.);
#5376=ORIENTED_EDGE('',*,*,#3934,.F.);
#5377=ORIENTED_EDGE('',*,*,#3919,.F.);
#5378=ORIENTED_EDGE('',*,*,#3928,.F.);
#5379=ORIENTED_EDGE('',*,*,#3731,.T.);
#5380=ORIENTED_EDGE('',*,*,#3727,.T.);
#5381=ORIENTED_EDGE('',*,*,#3724,.T.);
#5382=ORIENTED_EDGE('',*,*,#3721,.T.);
#5383=ORIENTED_EDGE('',*,*,#3718,.T.);
#5384=ORIENTED_EDGE('',*,*,#3715,.T.);
#5385=ORIENTED_EDGE('',*,*,#3931,.F.);
#5386=ORIENTED_EDGE('',*,*,#3824,.F.);
#5387=ORIENTED_EDGE('',*,*,#3936,.F.);
#5388=ORIENTED_EDGE('',*,*,#3933,.F.);
#5389=ORIENTED_EDGE('',*,*,#3929,.F.);
#5390=ORIENTED_EDGE('',*,*,#3826,.F.);
#5391=ORIENTED_EDGE('',*,*,#3932,.F.);
#5392=ORIENTED_EDGE('',*,*,#3925,.F.);
#5393=ORIENTED_EDGE('',*,*,#3937,.F.);
#5394=ORIENTED_EDGE('',*,*,#3938,.T.);
#5395=ORIENTED_EDGE('',*,*,#3939,.F.);
#5396=ORIENTED_EDGE('',*,*,#3938,.F.);
#5397=ORIENTED_EDGE('',*,*,#3940,.F.);
#5398=ORIENTED_EDGE('',*,*,#3941,.T.);
#5399=ORIENTED_EDGE('',*,*,#3942,.F.);
#5400=ORIENTED_EDGE('',*,*,#3941,.F.);
#5401=ORIENTED_EDGE('',*,*,#3943,.F.);
#5402=ORIENTED_EDGE('',*,*,#3944,.T.);
#5403=ORIENTED_EDGE('',*,*,#3945,.F.);
#5404=ORIENTED_EDGE('',*,*,#3944,.F.);
#5405=ORIENTED_EDGE('',*,*,#3946,.F.);
#5406=ORIENTED_EDGE('',*,*,#3947,.T.);
#5407=ORIENTED_EDGE('',*,*,#3948,.F.);
#5408=ORIENTED_EDGE('',*,*,#3947,.F.);
#5409=ORIENTED_EDGE('',*,*,#3949,.F.);
#5410=ORIENTED_EDGE('',*,*,#3950,.T.);
#5411=ORIENTED_EDGE('',*,*,#3951,.T.);
#5412=ORIENTED_EDGE('',*,*,#3952,.F.);
#5413=ORIENTED_EDGE('',*,*,#3953,.F.);
#5414=ORIENTED_EDGE('',*,*,#3954,.T.);
#5415=ORIENTED_EDGE('',*,*,#3955,.T.);
#5416=ORIENTED_EDGE('',*,*,#3950,.F.);
#5417=ORIENTED_EDGE('',*,*,#3956,.F.);
#5418=ORIENTED_EDGE('',*,*,#3957,.T.);
#5419=ORIENTED_EDGE('',*,*,#3958,.T.);
#5420=ORIENTED_EDGE('',*,*,#3954,.F.);
#5421=ORIENTED_EDGE('',*,*,#3959,.F.);
#5422=ORIENTED_EDGE('',*,*,#3960,.T.);
#5423=ORIENTED_EDGE('',*,*,#3961,.T.);
#5424=ORIENTED_EDGE('',*,*,#3957,.F.);
#5425=ORIENTED_EDGE('',*,*,#3962,.F.);
#5426=ORIENTED_EDGE('',*,*,#3963,.T.);
#5427=ORIENTED_EDGE('',*,*,#3964,.T.);
#5428=ORIENTED_EDGE('',*,*,#3960,.F.);
#5429=ORIENTED_EDGE('',*,*,#3965,.F.);
#5430=ORIENTED_EDGE('',*,*,#3952,.T.);
#5431=ORIENTED_EDGE('',*,*,#3966,.T.);
#5432=ORIENTED_EDGE('',*,*,#3963,.F.);
#5433=ORIENTED_EDGE('',*,*,#3966,.F.);
#5434=ORIENTED_EDGE('',*,*,#3951,.F.);
#5435=ORIENTED_EDGE('',*,*,#3955,.F.);
#5436=ORIENTED_EDGE('',*,*,#3958,.F.);
#5437=ORIENTED_EDGE('',*,*,#3961,.F.);
#5438=ORIENTED_EDGE('',*,*,#3964,.F.);
#5439=ORIENTED_EDGE('',*,*,#3967,.F.);
#5440=ORIENTED_EDGE('',*,*,#3968,.F.);
#5441=ORIENTED_EDGE('',*,*,#3969,.T.);
#5442=ORIENTED_EDGE('',*,*,#3970,.T.);
#5443=ORIENTED_EDGE('',*,*,#3971,.F.);
#5444=ORIENTED_EDGE('',*,*,#3972,.F.);
#5445=ORIENTED_EDGE('',*,*,#3973,.T.);
#5446=ORIENTED_EDGE('',*,*,#3974,.T.);
#5447=ORIENTED_EDGE('',*,*,#3969,.F.);
#5448=ORIENTED_EDGE('',*,*,#3975,.F.);
#5449=ORIENTED_EDGE('',*,*,#3976,.T.);
#5450=ORIENTED_EDGE('',*,*,#3977,.T.);
#5451=ORIENTED_EDGE('',*,*,#3973,.F.);
#5452=ORIENTED_EDGE('',*,*,#3978,.F.);
#5453=ORIENTED_EDGE('',*,*,#3979,.T.);
#5454=ORIENTED_EDGE('',*,*,#3980,.T.);
#5455=ORIENTED_EDGE('',*,*,#3976,.F.);
#5456=ORIENTED_EDGE('',*,*,#3981,.F.);
#5457=ORIENTED_EDGE('',*,*,#3982,.T.);
#5458=ORIENTED_EDGE('',*,*,#3983,.T.);
#5459=ORIENTED_EDGE('',*,*,#3979,.F.);
#5460=ORIENTED_EDGE('',*,*,#3984,.F.);
#5461=ORIENTED_EDGE('',*,*,#3971,.T.);
#5462=ORIENTED_EDGE('',*,*,#3985,.T.);
#5463=ORIENTED_EDGE('',*,*,#3982,.F.);
#5464=ORIENTED_EDGE('',*,*,#3985,.F.);
#5465=ORIENTED_EDGE('',*,*,#3970,.F.);
#5466=ORIENTED_EDGE('',*,*,#3974,.F.);
#5467=ORIENTED_EDGE('',*,*,#3977,.F.);
#5468=ORIENTED_EDGE('',*,*,#3980,.F.);
#5469=ORIENTED_EDGE('',*,*,#3983,.F.);
#5470=ORIENTED_EDGE('',*,*,#3986,.F.);
#5471=ORIENTED_EDGE('',*,*,#3986,.T.);
#5472=ORIENTED_EDGE('',*,*,#3987,.T.);
#5473=ORIENTED_EDGE('',*,*,#3988,.F.);
#5474=ORIENTED_EDGE('',*,*,#3987,.F.);
#5475=ORIENTED_EDGE('',*,*,#3967,.T.);
#5476=ORIENTED_EDGE('',*,*,#3989,.T.);
#5477=ORIENTED_EDGE('',*,*,#3990,.F.);
#5478=ORIENTED_EDGE('',*,*,#3989,.F.);
#5479=ORIENTED_EDGE('',*,*,#3991,.F.);
#5480=ORIENTED_EDGE('',*,*,#3992,.F.);
#5481=ORIENTED_EDGE('',*,*,#3993,.F.);
#5482=ORIENTED_EDGE('',*,*,#3994,.T.);
#5483=ORIENTED_EDGE('',*,*,#3995,.F.);
#5484=ORIENTED_EDGE('',*,*,#3996,.T.);
#5485=ORIENTED_EDGE('',*,*,#3997,.F.);
#5486=ORIENTED_EDGE('',*,*,#3998,.F.);
#5487=ORIENTED_EDGE('',*,*,#3999,.F.);
#5488=ORIENTED_EDGE('',*,*,#4000,.T.);
#5489=ORIENTED_EDGE('',*,*,#4001,.F.);
#5490=ORIENTED_EDGE('',*,*,#4002,.F.);
#5491=ORIENTED_EDGE('',*,*,#4003,.F.);
#5492=ORIENTED_EDGE('',*,*,#4004,.T.);
#5493=ORIENTED_EDGE('',*,*,#4005,.F.);
#5494=ORIENTED_EDGE('',*,*,#4006,.F.);
#5495=ORIENTED_EDGE('',*,*,#4007,.F.);
#5496=ORIENTED_EDGE('',*,*,#4008,.T.);
#5497=ORIENTED_EDGE('',*,*,#4009,.F.);
#5498=ORIENTED_EDGE('',*,*,#4010,.F.);
#5499=ORIENTED_EDGE('',*,*,#4011,.F.);
#5500=ORIENTED_EDGE('',*,*,#4012,.F.);
#5501=ORIENTED_EDGE('',*,*,#4013,.F.);
#5502=ORIENTED_EDGE('',*,*,#4014,.T.);
#5503=ORIENTED_EDGE('',*,*,#4015,.F.);
#5504=ORIENTED_EDGE('',*,*,#4016,.F.);
#5505=ORIENTED_EDGE('',*,*,#4017,.F.);
#5506=ORIENTED_EDGE('',*,*,#4018,.T.);
#5507=ORIENTED_EDGE('',*,*,#4019,.F.);
#5508=ORIENTED_EDGE('',*,*,#3988,.T.);
#5509=ORIENTED_EDGE('',*,*,#4020,.F.);
#5510=ORIENTED_EDGE('',*,*,#3990,.T.);
#5511=ORIENTED_EDGE('',*,*,#4021,.F.);
#5512=ORIENTED_EDGE('',*,*,#3994,.F.);
#5513=ORIENTED_EDGE('',*,*,#4022,.F.);
#5514=ORIENTED_EDGE('',*,*,#4008,.F.);
#5515=ORIENTED_EDGE('',*,*,#4023,.F.);
#5516=ORIENTED_EDGE('',*,*,#4014,.F.);
#5517=ORIENTED_EDGE('',*,*,#4024,.F.);
#5518=ORIENTED_EDGE('',*,*,#3996,.F.);
#5519=ORIENTED_EDGE('',*,*,#4025,.F.);
#5520=ORIENTED_EDGE('',*,*,#4018,.F.);
#5521=ORIENTED_EDGE('',*,*,#4026,.F.);
#5522=ORIENTED_EDGE('',*,*,#4000,.F.);
#5523=ORIENTED_EDGE('',*,*,#4027,.F.);
#5524=ORIENTED_EDGE('',*,*,#4028,.F.);
#5525=ORIENTED_EDGE('',*,*,#4029,.F.);
#5526=ORIENTED_EDGE('',*,*,#4004,.F.);
#5527=ORIENTED_EDGE('',*,*,#4030,.F.);
#5528=ORIENTED_EDGE('',*,*,#4031,.F.);
#5529=ORIENTED_EDGE('',*,*,#4032,.F.);
#5530=ORIENTED_EDGE('',*,*,#4028,.T.);
#5531=ORIENTED_EDGE('',*,*,#4033,.T.);
#5532=ORIENTED_EDGE('',*,*,#4034,.F.);
#5533=ORIENTED_EDGE('',*,*,#4035,.F.);
#5534=ORIENTED_EDGE('',*,*,#4036,.F.);
#5535=ORIENTED_EDGE('',*,*,#4037,.F.);
#5536=ORIENTED_EDGE('',*,*,#4038,.F.);
#5537=ORIENTED_EDGE('',*,*,#4005,.T.);
#5538=ORIENTED_EDGE('',*,*,#4029,.T.);
#5539=ORIENTED_EDGE('',*,*,#4032,.T.);
#5540=ORIENTED_EDGE('',*,*,#4039,.T.);
#5541=ORIENTED_EDGE('',*,*,#4040,.F.);
#5542=ORIENTED_EDGE('',*,*,#4041,.F.);
#5543=ORIENTED_EDGE('',*,*,#4042,.F.);
#5544=ORIENTED_EDGE('',*,*,#4043,.F.);
#5545=ORIENTED_EDGE('',*,*,#4044,.F.);
#5546=ORIENTED_EDGE('',*,*,#4045,.T.);
#5547=ORIENTED_EDGE('',*,*,#4001,.T.);
#5548=ORIENTED_EDGE('',*,*,#4026,.T.);
#5549=ORIENTED_EDGE('',*,*,#4017,.T.);
#5550=ORIENTED_EDGE('',*,*,#4046,.T.);
#5551=ORIENTED_EDGE('',*,*,#4047,.F.);
#5552=ORIENTED_EDGE('',*,*,#4048,.F.);
#5553=ORIENTED_EDGE('',*,*,#4049,.F.);
#5554=ORIENTED_EDGE('',*,*,#4050,.F.);
#5555=ORIENTED_EDGE('',*,*,#4051,.F.);
#5556=ORIENTED_EDGE('',*,*,#4052,.T.);
#5557=ORIENTED_EDGE('',*,*,#3997,.T.);
#5558=ORIENTED_EDGE('',*,*,#4024,.T.);
#5559=ORIENTED_EDGE('',*,*,#4013,.T.);
#5560=ORIENTED_EDGE('',*,*,#4053,.T.);
#5561=ORIENTED_EDGE('',*,*,#4054,.F.);
#5562=ORIENTED_EDGE('',*,*,#4055,.F.);
#5563=ORIENTED_EDGE('',*,*,#4056,.F.);
#5564=ORIENTED_EDGE('',*,*,#4057,.F.);
#5565=ORIENTED_EDGE('',*,*,#4058,.F.);
#5566=ORIENTED_EDGE('',*,*,#4059,.T.);
#5567=ORIENTED_EDGE('',*,*,#3991,.T.);
#5568=ORIENTED_EDGE('',*,*,#4021,.T.);
#5569=ORIENTED_EDGE('',*,*,#4007,.T.);
#5570=ORIENTED_EDGE('',*,*,#4060,.F.);
#5571=ORIENTED_EDGE('',*,*,#4061,.T.);
#5572=ORIENTED_EDGE('',*,*,#4062,.T.);
#5573=ORIENTED_EDGE('',*,*,#4063,.T.);
#5574=ORIENTED_EDGE('',*,*,#4064,.F.);
#5575=ORIENTED_EDGE('',*,*,#4006,.T.);
#5576=ORIENTED_EDGE('',*,*,#4045,.F.);
#5577=ORIENTED_EDGE('',*,*,#4065,.T.);
#5578=ORIENTED_EDGE('',*,*,#4033,.F.);
#5579=ORIENTED_EDGE('',*,*,#4066,.T.);
#5580=ORIENTED_EDGE('',*,*,#4039,.F.);
#5581=ORIENTED_EDGE('',*,*,#4031,.T.);
#5582=ORIENTED_EDGE('',*,*,#4067,.F.);
#5583=ORIENTED_EDGE('',*,*,#4068,.T.);
#5584=ORIENTED_EDGE('',*,*,#4046,.F.);
#5585=ORIENTED_EDGE('',*,*,#4016,.T.);
#5586=ORIENTED_EDGE('',*,*,#4069,.F.);
#5587=ORIENTED_EDGE('',*,*,#4070,.T.);
#5588=ORIENTED_EDGE('',*,*,#4053,.F.);
#5589=ORIENTED_EDGE('',*,*,#4012,.T.);
#5590=ORIENTED_EDGE('',*,*,#4071,.F.);
#5591=ORIENTED_EDGE('',*,*,#4072,.T.);
#5592=ORIENTED_EDGE('',*,*,#4073,.T.);
#5593=ORIENTED_EDGE('',*,*,#4060,.T.);
#5594=ORIENTED_EDGE('',*,*,#4010,.T.);
#5595=ORIENTED_EDGE('',*,*,#4074,.T.);
#5596=ORIENTED_EDGE('',*,*,#4075,.F.);
#5597=ORIENTED_EDGE('',*,*,#4076,.T.);
#5598=ORIENTED_EDGE('',*,*,#4077,.F.);
#5599=ORIENTED_EDGE('',*,*,#4078,.T.);
#5600=ORIENTED_EDGE('',*,*,#4079,.F.);
#5601=ORIENTED_EDGE('',*,*,#4080,.T.);
#5602=ORIENTED_EDGE('',*,*,#4081,.F.);
#5603=ORIENTED_EDGE('',*,*,#4082,.T.);
#5604=ORIENTED_EDGE('',*,*,#3992,.T.);
#5605=ORIENTED_EDGE('',*,*,#4064,.T.);
#5606=ORIENTED_EDGE('',*,*,#4083,.T.);
#5607=ORIENTED_EDGE('',*,*,#4084,.T.);
#5608=ORIENTED_EDGE('',*,*,#4085,.F.);
#5609=ORIENTED_EDGE('',*,*,#3998,.T.);
#5610=ORIENTED_EDGE('',*,*,#4059,.F.);
#5611=ORIENTED_EDGE('',*,*,#4086,.T.);
#5612=ORIENTED_EDGE('',*,*,#4087,.F.);
#5613=ORIENTED_EDGE('',*,*,#4002,.T.);
#5614=ORIENTED_EDGE('',*,*,#4052,.F.);
#5615=ORIENTED_EDGE('',*,*,#4088,.T.);
#5616=ORIENTED_EDGE('',*,*,#4089,.F.);
#5617=ORIENTED_EDGE('',*,*,#4090,.T.);
#5618=ORIENTED_EDGE('',*,*,#4091,.T.);
#5619=ORIENTED_EDGE('',*,*,#4092,.T.);
#5620=ORIENTED_EDGE('',*,*,#4093,.T.);
#5621=ORIENTED_EDGE('',*,*,#4094,.T.);
#5622=ORIENTED_EDGE('',*,*,#4095,.F.);
#5623=ORIENTED_EDGE('',*,*,#4096,.F.);
#5624=ORIENTED_EDGE('',*,*,#4097,.T.);
#5625=ORIENTED_EDGE('',*,*,#4020,.T.);
#5626=ORIENTED_EDGE('',*,*,#4097,.F.);
#5627=ORIENTED_EDGE('',*,*,#4098,.F.);
#5628=ORIENTED_EDGE('',*,*,#4099,.T.);
#5629=ORIENTED_EDGE('',*,*,#4019,.T.);
#5630=ORIENTED_EDGE('',*,*,#4099,.F.);
#5631=ORIENTED_EDGE('',*,*,#4100,.F.);
#5632=ORIENTED_EDGE('',*,*,#4095,.T.);
#5633=ORIENTED_EDGE('',*,*,#4101,.F.);
#5634=ORIENTED_EDGE('',*,*,#4102,.F.);
#5635=ORIENTED_EDGE('',*,*,#4103,.F.);
#5636=ORIENTED_EDGE('',*,*,#4104,.F.);
#5637=ORIENTED_EDGE('',*,*,#4034,.T.);
#5638=ORIENTED_EDGE('',*,*,#4065,.F.);
#5639=ORIENTED_EDGE('',*,*,#4044,.T.);
#5640=ORIENTED_EDGE('',*,*,#4105,.T.);
#5641=ORIENTED_EDGE('',*,*,#4100,.T.);
#5642=ORIENTED_EDGE('',*,*,#4106,.T.);
#5643=ORIENTED_EDGE('',*,*,#4107,.T.);
#5644=ORIENTED_EDGE('',*,*,#4090,.F.);
#5645=ORIENTED_EDGE('',*,*,#4035,.T.);
#5646=ORIENTED_EDGE('',*,*,#4105,.F.);
#5647=ORIENTED_EDGE('',*,*,#4043,.T.);
#5648=ORIENTED_EDGE('',*,*,#4108,.F.);
#5649=ORIENTED_EDGE('',*,*,#4104,.T.);
#5650=ORIENTED_EDGE('',*,*,#4109,.F.);
#5651=ORIENTED_EDGE('',*,*,#4110,.F.);
#5652=ORIENTED_EDGE('',*,*,#4106,.F.);
#5653=ORIENTED_EDGE('',*,*,#4036,.T.);
#5654=ORIENTED_EDGE('',*,*,#4108,.T.);
#5655=ORIENTED_EDGE('',*,*,#4042,.T.);
#5656=ORIENTED_EDGE('',*,*,#4111,.T.);
#5657=ORIENTED_EDGE('',*,*,#3939,.T.);
#5658=ORIENTED_EDGE('',*,*,#3948,.T.);
#5659=ORIENTED_EDGE('',*,*,#4096,.T.);
#5660=ORIENTED_EDGE('',*,*,#4103,.T.);
#5661=ORIENTED_EDGE('',*,*,#4112,.T.);
#5662=ORIENTED_EDGE('',*,*,#4113,.T.);
#5663=ORIENTED_EDGE('',*,*,#4109,.T.);
#5664=ORIENTED_EDGE('',*,*,#4037,.T.);
#5665=ORIENTED_EDGE('',*,*,#4111,.F.);
#5666=ORIENTED_EDGE('',*,*,#4041,.T.);
#5667=ORIENTED_EDGE('',*,*,#4114,.F.);
#5668=ORIENTED_EDGE('',*,*,#4038,.T.);
#5669=ORIENTED_EDGE('',*,*,#4114,.T.);
#5670=ORIENTED_EDGE('',*,*,#4040,.T.);
#5671=ORIENTED_EDGE('',*,*,#4066,.F.);
#5672=ORIENTED_EDGE('',*,*,#4101,.T.);
#5673=ORIENTED_EDGE('',*,*,#4094,.F.);
#5674=ORIENTED_EDGE('',*,*,#4115,.T.);
#5675=ORIENTED_EDGE('',*,*,#4116,.T.);
#5676=ORIENTED_EDGE('',*,*,#4003,.T.);
#5677=ORIENTED_EDGE('',*,*,#4089,.T.);
#5678=ORIENTED_EDGE('',*,*,#4117,.F.);
#5679=ORIENTED_EDGE('',*,*,#4118,.F.);
#5680=ORIENTED_EDGE('',*,*,#4119,.F.);
#5681=ORIENTED_EDGE('',*,*,#4120,.F.);
#5682=ORIENTED_EDGE('',*,*,#4121,.F.);
#5683=ORIENTED_EDGE('',*,*,#4067,.T.);
#5684=ORIENTED_EDGE('',*,*,#4030,.T.);
#5685=ORIENTED_EDGE('',*,*,#4027,.T.);
#5686=ORIENTED_EDGE('',*,*,#4117,.T.);
#5687=ORIENTED_EDGE('',*,*,#4088,.F.);
#5688=ORIENTED_EDGE('',*,*,#4051,.T.);
#5689=ORIENTED_EDGE('',*,*,#4122,.T.);
#5690=ORIENTED_EDGE('',*,*,#4118,.T.);
#5691=ORIENTED_EDGE('',*,*,#4122,.F.);
#5692=ORIENTED_EDGE('',*,*,#4050,.T.);
#5693=ORIENTED_EDGE('',*,*,#4123,.F.);
#5694=ORIENTED_EDGE('',*,*,#4119,.T.);
#5695=ORIENTED_EDGE('',*,*,#4123,.T.);
#5696=ORIENTED_EDGE('',*,*,#4049,.T.);
#5697=ORIENTED_EDGE('',*,*,#4124,.T.);
#5698=ORIENTED_EDGE('',*,*,#4120,.T.);
#5699=ORIENTED_EDGE('',*,*,#4124,.F.);
#5700=ORIENTED_EDGE('',*,*,#4048,.T.);
#5701=ORIENTED_EDGE('',*,*,#4125,.F.);
#5702=ORIENTED_EDGE('',*,*,#4121,.T.);
#5703=ORIENTED_EDGE('',*,*,#4125,.T.);
#5704=ORIENTED_EDGE('',*,*,#4047,.T.);
#5705=ORIENTED_EDGE('',*,*,#4068,.F.);
#5706=ORIENTED_EDGE('',*,*,#3999,.T.);
#5707=ORIENTED_EDGE('',*,*,#4087,.T.);
#5708=ORIENTED_EDGE('',*,*,#4126,.F.);
#5709=ORIENTED_EDGE('',*,*,#4127,.F.);
#5710=ORIENTED_EDGE('',*,*,#4128,.F.);
#5711=ORIENTED_EDGE('',*,*,#4129,.F.);
#5712=ORIENTED_EDGE('',*,*,#4130,.F.);
#5713=ORIENTED_EDGE('',*,*,#4069,.T.);
#5714=ORIENTED_EDGE('',*,*,#4015,.T.);
#5715=ORIENTED_EDGE('',*,*,#4025,.T.);
#5716=ORIENTED_EDGE('',*,*,#4126,.T.);
#5717=ORIENTED_EDGE('',*,*,#4086,.F.);
#5718=ORIENTED_EDGE('',*,*,#4058,.T.);
#5719=ORIENTED_EDGE('',*,*,#4131,.T.);
#5720=ORIENTED_EDGE('',*,*,#4127,.T.);
#5721=ORIENTED_EDGE('',*,*,#4131,.F.);
#5722=ORIENTED_EDGE('',*,*,#4057,.T.);
#5723=ORIENTED_EDGE('',*,*,#4132,.F.);
#5724=ORIENTED_EDGE('',*,*,#4128,.T.);
#5725=ORIENTED_EDGE('',*,*,#4132,.T.);
#5726=ORIENTED_EDGE('',*,*,#4056,.T.);
#5727=ORIENTED_EDGE('',*,*,#4133,.T.);
#5728=ORIENTED_EDGE('',*,*,#3942,.T.);
#5729=ORIENTED_EDGE('',*,*,#3945,.T.);
#5730=ORIENTED_EDGE('',*,*,#4098,.T.);
#5731=ORIENTED_EDGE('',*,*,#4129,.T.);
#5732=ORIENTED_EDGE('',*,*,#4133,.F.);
#5733=ORIENTED_EDGE('',*,*,#4055,.T.);
#5734=ORIENTED_EDGE('',*,*,#4134,.F.);
#5735=ORIENTED_EDGE('',*,*,#4130,.T.);
#5736=ORIENTED_EDGE('',*,*,#4134,.T.);
#5737=ORIENTED_EDGE('',*,*,#4054,.T.);
#5738=ORIENTED_EDGE('',*,*,#4070,.F.);
#5739=ORIENTED_EDGE('',*,*,#3995,.T.);
#5740=ORIENTED_EDGE('',*,*,#4085,.T.);
#5741=ORIENTED_EDGE('',*,*,#4135,.F.);
#5742=ORIENTED_EDGE('',*,*,#4136,.F.);
#5743=ORIENTED_EDGE('',*,*,#4137,.F.);
#5744=ORIENTED_EDGE('',*,*,#4138,.F.);
#5745=ORIENTED_EDGE('',*,*,#4139,.F.);
#5746=ORIENTED_EDGE('',*,*,#4071,.T.);
#5747=ORIENTED_EDGE('',*,*,#4011,.T.);
#5748=ORIENTED_EDGE('',*,*,#4023,.T.);
#5749=ORIENTED_EDGE('',*,*,#4135,.T.);
#5750=ORIENTED_EDGE('',*,*,#4084,.F.);
#5751=ORIENTED_EDGE('',*,*,#4140,.T.);
#5752=ORIENTED_EDGE('',*,*,#4141,.T.);
#5753=ORIENTED_EDGE('',*,*,#4136,.T.);
#5754=ORIENTED_EDGE('',*,*,#4141,.F.);
#5755=ORIENTED_EDGE('',*,*,#4142,.F.);
#5756=ORIENTED_EDGE('',*,*,#4143,.F.);
#5757=ORIENTED_EDGE('',*,*,#4137,.T.);
#5758=ORIENTED_EDGE('',*,*,#4143,.T.);
#5759=ORIENTED_EDGE('',*,*,#4144,.T.);
#5760=ORIENTED_EDGE('',*,*,#4145,.T.);
#5761=ORIENTED_EDGE('',*,*,#4139,.T.);
#5762=ORIENTED_EDGE('',*,*,#4146,.T.);
#5763=ORIENTED_EDGE('',*,*,#4147,.T.);
#5764=ORIENTED_EDGE('',*,*,#4072,.F.);
#5765=ORIENTED_EDGE('',*,*,#4138,.T.);
#5766=ORIENTED_EDGE('',*,*,#4145,.F.);
#5767=ORIENTED_EDGE('',*,*,#4148,.F.);
#5768=ORIENTED_EDGE('',*,*,#4146,.F.);
#5769=ORIENTED_EDGE('',*,*,#4149,.T.);
#5770=ORIENTED_EDGE('',*,*,#4150,.T.);
#5771=ORIENTED_EDGE('',*,*,#4148,.T.);
#5772=ORIENTED_EDGE('',*,*,#4151,.T.);
#5773=ORIENTED_EDGE('',*,*,#4152,.T.);
#5774=ORIENTED_EDGE('',*,*,#4153,.T.);
#5775=ORIENTED_EDGE('',*,*,#4142,.T.);
#5776=ORIENTED_EDGE('',*,*,#4154,.T.);
#5777=ORIENTED_EDGE('',*,*,#4155,.T.);
#5778=ORIENTED_EDGE('',*,*,#4149,.F.);
#5779=ORIENTED_EDGE('',*,*,#4144,.F.);
#5780=ORIENTED_EDGE('',*,*,#4155,.F.);
#5781=ORIENTED_EDGE('',*,*,#4062,.F.);
#5782=ORIENTED_EDGE('',*,*,#4083,.F.);
#5783=ORIENTED_EDGE('',*,*,#4063,.F.);
#5784=ORIENTED_EDGE('',*,*,#4154,.F.);
#5785=ORIENTED_EDGE('',*,*,#4140,.F.);
#5786=ORIENTED_EDGE('',*,*,#4156,.T.);
#5787=ORIENTED_EDGE('',*,*,#4110,.T.);
#5788=ORIENTED_EDGE('',*,*,#4157,.T.);
#5789=ORIENTED_EDGE('',*,*,#4157,.F.);
#5790=ORIENTED_EDGE('',*,*,#4113,.F.);
#5791=ORIENTED_EDGE('',*,*,#4153,.F.);
#5792=ORIENTED_EDGE('',*,*,#4158,.F.);
#5793=ORIENTED_EDGE('',*,*,#4091,.F.);
#5794=ORIENTED_EDGE('',*,*,#4107,.F.);
#5795=ORIENTED_EDGE('',*,*,#4156,.F.);
#5796=ORIENTED_EDGE('',*,*,#4159,.F.);
#5797=ORIENTED_EDGE('',*,*,#4093,.F.);
#5798=ORIENTED_EDGE('',*,*,#4160,.F.);
#5799=ORIENTED_EDGE('',*,*,#4152,.F.);
#5800=ORIENTED_EDGE('',*,*,#4115,.F.);
#5801=ORIENTED_EDGE('',*,*,#4102,.T.);
#5802=ORIENTED_EDGE('',*,*,#4116,.F.);
#5803=ORIENTED_EDGE('',*,*,#4151,.F.);
#5804=ORIENTED_EDGE('',*,*,#4112,.F.);
#5805=ORIENTED_EDGE('',*,*,#4073,.F.);
#5806=ORIENTED_EDGE('',*,*,#4147,.F.);
#5807=ORIENTED_EDGE('',*,*,#4150,.F.);
#5808=ORIENTED_EDGE('',*,*,#4061,.F.);
#5809=ORIENTED_EDGE('',*,*,#4159,.T.);
#5810=ORIENTED_EDGE('',*,*,#4158,.T.);
#5811=ORIENTED_EDGE('',*,*,#4160,.T.);
#5812=ORIENTED_EDGE('',*,*,#4092,.F.);
#5813=ORIENTED_EDGE('',*,*,#4161,.F.);
#5814=ORIENTED_EDGE('',*,*,#4162,.F.);
#5815=ORIENTED_EDGE('',*,*,#4163,.F.);
#5816=ORIENTED_EDGE('',*,*,#4164,.F.);
#5817=ORIENTED_EDGE('',*,*,#4165,.F.);
#5818=ORIENTED_EDGE('',*,*,#4166,.F.);
#5819=ORIENTED_EDGE('',*,*,#4167,.F.);
#5820=ORIENTED_EDGE('',*,*,#4168,.F.);
#5821=ORIENTED_EDGE('',*,*,#4169,.F.);
#5822=ORIENTED_EDGE('',*,*,#4161,.T.);
#5823=ORIENTED_EDGE('',*,*,#4170,.T.);
#5824=ORIENTED_EDGE('',*,*,#4168,.T.);
#5825=ORIENTED_EDGE('',*,*,#4171,.T.);
#5826=ORIENTED_EDGE('',*,*,#4081,.T.);
#5827=ORIENTED_EDGE('',*,*,#4172,.T.);
#5828=ORIENTED_EDGE('',*,*,#4169,.T.);
#5829=ORIENTED_EDGE('',*,*,#4173,.T.);
#5830=ORIENTED_EDGE('',*,*,#4174,.F.);
#5831=ORIENTED_EDGE('',*,*,#4175,.F.);
#5832=ORIENTED_EDGE('',*,*,#4176,.F.);
#5833=ORIENTED_EDGE('',*,*,#4175,.T.);
#5834=ORIENTED_EDGE('',*,*,#4177,.T.);
#5835=ORIENTED_EDGE('',*,*,#4165,.T.);
#5836=ORIENTED_EDGE('',*,*,#4178,.T.);
#5837=ORIENTED_EDGE('',*,*,#4167,.T.);
#5838=ORIENTED_EDGE('',*,*,#4179,.T.);
#5839=ORIENTED_EDGE('',*,*,#4176,.T.);
#5840=ORIENTED_EDGE('',*,*,#4180,.T.);
#5841=ORIENTED_EDGE('',*,*,#4079,.T.);
#5842=ORIENTED_EDGE('',*,*,#4181,.T.);
#5843=ORIENTED_EDGE('',*,*,#4174,.T.);
#5844=ORIENTED_EDGE('',*,*,#4182,.T.);
#5845=ORIENTED_EDGE('',*,*,#4077,.T.);
#5846=ORIENTED_EDGE('',*,*,#4183,.T.);
#5847=ORIENTED_EDGE('',*,*,#4166,.T.);
#5848=ORIENTED_EDGE('',*,*,#4184,.T.);
#5849=ORIENTED_EDGE('',*,*,#4164,.T.);
#5850=ORIENTED_EDGE('',*,*,#4185,.T.);
#5851=ORIENTED_EDGE('',*,*,#4162,.T.);
#5852=ORIENTED_EDGE('',*,*,#4186,.T.);
#5853=ORIENTED_EDGE('',*,*,#4075,.T.);
#5854=ORIENTED_EDGE('',*,*,#4187,.T.);
#5855=ORIENTED_EDGE('',*,*,#4163,.T.);
#5856=ORIENTED_EDGE('',*,*,#4188,.T.);
#5857=ORIENTED_EDGE('',*,*,#4182,.F.);
#5858=ORIENTED_EDGE('',*,*,#4179,.F.);
#5859=ORIENTED_EDGE('',*,*,#4172,.F.);
#5860=ORIENTED_EDGE('',*,*,#4080,.F.);
#5861=ORIENTED_EDGE('',*,*,#3993,.T.);
#5862=ORIENTED_EDGE('',*,*,#4082,.F.);
#5863=ORIENTED_EDGE('',*,*,#4173,.F.);
#5864=ORIENTED_EDGE('',*,*,#4170,.F.);
#5865=ORIENTED_EDGE('',*,*,#4187,.F.);
#5866=ORIENTED_EDGE('',*,*,#4074,.F.);
#5867=ORIENTED_EDGE('',*,*,#4009,.T.);
#5868=ORIENTED_EDGE('',*,*,#4022,.T.);
#5869=ORIENTED_EDGE('',*,*,#4178,.F.);
#5870=ORIENTED_EDGE('',*,*,#4186,.F.);
#5871=ORIENTED_EDGE('',*,*,#4171,.F.);
#5872=ORIENTED_EDGE('',*,*,#4180,.F.);
#5873=ORIENTED_EDGE('',*,*,#3968,.T.);
#5874=ORIENTED_EDGE('',*,*,#3984,.T.);
#5875=ORIENTED_EDGE('',*,*,#3981,.T.);
#5876=ORIENTED_EDGE('',*,*,#3978,.T.);
#5877=ORIENTED_EDGE('',*,*,#3975,.T.);
#5878=ORIENTED_EDGE('',*,*,#3972,.T.);
#5879=ORIENTED_EDGE('',*,*,#3949,.T.);
#5880=ORIENTED_EDGE('',*,*,#3965,.T.);
#5881=ORIENTED_EDGE('',*,*,#3962,.T.);
#5882=ORIENTED_EDGE('',*,*,#3959,.T.);
#5883=ORIENTED_EDGE('',*,*,#3956,.T.);
#5884=ORIENTED_EDGE('',*,*,#3953,.T.);
#5885=ORIENTED_EDGE('',*,*,#3946,.T.);
#5886=ORIENTED_EDGE('',*,*,#3943,.T.);
#5887=ORIENTED_EDGE('',*,*,#3940,.T.);
#5888=ORIENTED_EDGE('',*,*,#3937,.T.);
#5889=ORIENTED_EDGE('',*,*,#4183,.F.);
#5890=ORIENTED_EDGE('',*,*,#4076,.F.);
#5891=ORIENTED_EDGE('',*,*,#4188,.F.);
#5892=ORIENTED_EDGE('',*,*,#4185,.F.);
#5893=ORIENTED_EDGE('',*,*,#4181,.F.);
#5894=ORIENTED_EDGE('',*,*,#4078,.F.);
#5895=ORIENTED_EDGE('',*,*,#4184,.F.);
#5896=ORIENTED_EDGE('',*,*,#4177,.F.);
#5897=ORIENTED_EDGE('',*,*,#4189,.F.);
#5898=ORIENTED_EDGE('',*,*,#4190,.T.);
#5899=ORIENTED_EDGE('',*,*,#4191,.F.);
#5900=ORIENTED_EDGE('',*,*,#4190,.F.);
#5901=ORIENTED_EDGE('',*,*,#4192,.F.);
#5902=ORIENTED_EDGE('',*,*,#4193,.T.);
#5903=ORIENTED_EDGE('',*,*,#4194,.F.);
#5904=ORIENTED_EDGE('',*,*,#4193,.F.);
#5905=ORIENTED_EDGE('',*,*,#4195,.T.);
#5906=ORIENTED_EDGE('',*,*,#4196,.T.);
#5907=ORIENTED_EDGE('',*,*,#4197,.F.);
#5908=ORIENTED_EDGE('',*,*,#4198,.T.);
#5909=ORIENTED_EDGE('',*,*,#4195,.F.);
#5910=ORIENTED_EDGE('',*,*,#4198,.F.);
#5911=ORIENTED_EDGE('',*,*,#4197,.T.);
#5912=ORIENTED_EDGE('',*,*,#4199,.T.);
#5913=ORIENTED_EDGE('',*,*,#4200,.T.);
#5914=ORIENTED_EDGE('',*,*,#4201,.F.);
#5915=ORIENTED_EDGE('',*,*,#4202,.T.);
#5916=ORIENTED_EDGE('',*,*,#4199,.F.);
#5917=ORIENTED_EDGE('',*,*,#4202,.F.);
#5918=ORIENTED_EDGE('',*,*,#4201,.T.);
#5919=ORIENTED_EDGE('',*,*,#4203,.T.);
#5920=ORIENTED_EDGE('',*,*,#4204,.T.);
#5921=ORIENTED_EDGE('',*,*,#4205,.F.);
#5922=ORIENTED_EDGE('',*,*,#4206,.T.);
#5923=ORIENTED_EDGE('',*,*,#4203,.F.);
#5924=ORIENTED_EDGE('',*,*,#4206,.F.);
#5925=ORIENTED_EDGE('',*,*,#4205,.T.);
#5926=ORIENTED_EDGE('',*,*,#4207,.T.);
#5927=ORIENTED_EDGE('',*,*,#4208,.T.);
#5928=ORIENTED_EDGE('',*,*,#4209,.F.);
#5929=ORIENTED_EDGE('',*,*,#4210,.T.);
#5930=ORIENTED_EDGE('',*,*,#4207,.F.);
#5931=ORIENTED_EDGE('',*,*,#4210,.F.);
#5932=ORIENTED_EDGE('',*,*,#4209,.T.);
#5933=ORIENTED_EDGE('',*,*,#4196,.F.);
#5934=ORIENTED_EDGE('',*,*,#4211,.T.);
#5935=ORIENTED_EDGE('',*,*,#4212,.F.);
#5936=ORIENTED_EDGE('',*,*,#4211,.F.);
#5937=ORIENTED_EDGE('',*,*,#4200,.F.);
#5938=ORIENTED_EDGE('',*,*,#4213,.T.);
#5939=ORIENTED_EDGE('',*,*,#4214,.F.);
#5940=ORIENTED_EDGE('',*,*,#4213,.F.);
#5941=ORIENTED_EDGE('',*,*,#4204,.F.);
#5942=ORIENTED_EDGE('',*,*,#4215,.T.);
#5943=ORIENTED_EDGE('',*,*,#4216,.F.);
#5944=ORIENTED_EDGE('',*,*,#4215,.F.);
#5945=ORIENTED_EDGE('',*,*,#4208,.F.);
#5946=ORIENTED_EDGE('',*,*,#4217,.T.);
#5947=ORIENTED_EDGE('',*,*,#4218,.F.);
#5948=ORIENTED_EDGE('',*,*,#4217,.F.);
#5949=ORIENTED_EDGE('',*,*,#4219,.T.);
#5950=ORIENTED_EDGE('',*,*,#4220,.T.);
#5951=ORIENTED_EDGE('',*,*,#4221,.T.);
#5952=ORIENTED_EDGE('',*,*,#4222,.T.);
#5953=ORIENTED_EDGE('',*,*,#4223,.T.);
#5954=ORIENTED_EDGE('',*,*,#4224,.T.);
#5955=ORIENTED_EDGE('',*,*,#4219,.F.);
#5956=ORIENTED_EDGE('',*,*,#4225,.T.);
#5957=ORIENTED_EDGE('',*,*,#4226,.T.);
#5958=ORIENTED_EDGE('',*,*,#4227,.T.);
#5959=ORIENTED_EDGE('',*,*,#4223,.F.);
#5960=ORIENTED_EDGE('',*,*,#4228,.T.);
#5961=ORIENTED_EDGE('',*,*,#4229,.T.);
#5962=ORIENTED_EDGE('',*,*,#4230,.T.);
#5963=ORIENTED_EDGE('',*,*,#4226,.F.);
#5964=ORIENTED_EDGE('',*,*,#4231,.T.);
#5965=ORIENTED_EDGE('',*,*,#4232,.T.);
#5966=ORIENTED_EDGE('',*,*,#4233,.T.);
#5967=ORIENTED_EDGE('',*,*,#4229,.F.);
#5968=ORIENTED_EDGE('',*,*,#4234,.T.);
#5969=ORIENTED_EDGE('',*,*,#4235,.T.);
#5970=ORIENTED_EDGE('',*,*,#4236,.T.);
#5971=ORIENTED_EDGE('',*,*,#4232,.F.);
#5972=ORIENTED_EDGE('',*,*,#4237,.T.);
#5973=ORIENTED_EDGE('',*,*,#4238,.T.);
#5974=ORIENTED_EDGE('',*,*,#4239,.T.);
#5975=ORIENTED_EDGE('',*,*,#4235,.F.);
#5976=ORIENTED_EDGE('',*,*,#4240,.T.);
#5977=ORIENTED_EDGE('',*,*,#4221,.F.);
#5978=ORIENTED_EDGE('',*,*,#4241,.T.);
#5979=ORIENTED_EDGE('',*,*,#4238,.F.);
#5980=ORIENTED_EDGE('',*,*,#4242,.T.);
#5981=ORIENTED_EDGE('',*,*,#4236,.F.);
#5982=ORIENTED_EDGE('',*,*,#4243,.F.);
#5983=ORIENTED_EDGE('',*,*,#4244,.F.);
#5984=ORIENTED_EDGE('',*,*,#4245,.F.);
#5985=ORIENTED_EDGE('',*,*,#4239,.F.);
#5986=ORIENTED_EDGE('',*,*,#4246,.T.);
#5987=ORIENTED_EDGE('',*,*,#4247,.T.);
#5988=ORIENTED_EDGE('',*,*,#4243,.T.);
#5989=ORIENTED_EDGE('',*,*,#4241,.F.);
#5990=ORIENTED_EDGE('',*,*,#4248,.F.);
#5991=ORIENTED_EDGE('',*,*,#4249,.F.);
#5992=ORIENTED_EDGE('',*,*,#4246,.F.);
#5993=ORIENTED_EDGE('',*,*,#4220,.F.);
#5994=ORIENTED_EDGE('',*,*,#4250,.T.);
#5995=ORIENTED_EDGE('',*,*,#4251,.T.);
#5996=ORIENTED_EDGE('',*,*,#4248,.T.);
#5997=ORIENTED_EDGE('',*,*,#4222,.F.);
#5998=ORIENTED_EDGE('',*,*,#4242,.F.);
#5999=ORIENTED_EDGE('',*,*,#4240,.F.);
#6000=ORIENTED_EDGE('',*,*,#4237,.F.);
#6001=ORIENTED_EDGE('',*,*,#4234,.F.);
#6002=ORIENTED_EDGE('',*,*,#4231,.F.);
#6003=ORIENTED_EDGE('',*,*,#4228,.F.);
#6004=ORIENTED_EDGE('',*,*,#4225,.F.);
#6005=ORIENTED_EDGE('',*,*,#4189,.T.);
#6006=ORIENTED_EDGE('',*,*,#4192,.T.);
#6007=ORIENTED_EDGE('',*,*,#4224,.F.);
#6008=ORIENTED_EDGE('',*,*,#4252,.F.);
#6009=ORIENTED_EDGE('',*,*,#4253,.F.);
#6010=ORIENTED_EDGE('',*,*,#4250,.F.);
#6011=ORIENTED_EDGE('',*,*,#4233,.F.);
#6012=ORIENTED_EDGE('',*,*,#4245,.T.);
#6013=ORIENTED_EDGE('',*,*,#4254,.T.);
#6014=ORIENTED_EDGE('',*,*,#4255,.T.);
#6015=ORIENTED_EDGE('',*,*,#4227,.F.);
#6016=ORIENTED_EDGE('',*,*,#4256,.T.);
#6017=ORIENTED_EDGE('',*,*,#4257,.T.);
#6018=ORIENTED_EDGE('',*,*,#4252,.T.);
#6019=ORIENTED_EDGE('',*,*,#4251,.F.);
#6020=ORIENTED_EDGE('',*,*,#4253,.T.);
#6021=ORIENTED_EDGE('',*,*,#4257,.F.);
#6022=ORIENTED_EDGE('',*,*,#4258,.T.);
#6023=ORIENTED_EDGE('',*,*,#4254,.F.);
#6024=ORIENTED_EDGE('',*,*,#4244,.T.);
#6025=ORIENTED_EDGE('',*,*,#4247,.F.);
#6026=ORIENTED_EDGE('',*,*,#4249,.T.);
#6027=ORIENTED_EDGE('',*,*,#4191,.T.);
#6028=ORIENTED_EDGE('',*,*,#4194,.T.);
#6029=ORIENTED_EDGE('',*,*,#4212,.T.);
#6030=ORIENTED_EDGE('',*,*,#4214,.T.);
#6031=ORIENTED_EDGE('',*,*,#4216,.T.);
#6032=ORIENTED_EDGE('',*,*,#4218,.T.);
#6033=ORIENTED_EDGE('',*,*,#4230,.F.);
#6034=ORIENTED_EDGE('',*,*,#4255,.F.);
#6035=ORIENTED_EDGE('',*,*,#4258,.F.);
#6036=ORIENTED_EDGE('',*,*,#4256,.F.);
#6037=ORIENTED_EDGE('',*,*,#4259,.F.);
#6038=ORIENTED_EDGE('',*,*,#4260,.T.);
#6039=ORIENTED_EDGE('',*,*,#4261,.T.);
#6040=ORIENTED_EDGE('',*,*,#4262,.T.);
#6041=ORIENTED_EDGE('',*,*,#4263,.F.);
#6042=ORIENTED_EDGE('',*,*,#4264,.T.);
#6043=ORIENTED_EDGE('',*,*,#4259,.T.);
#6044=ORIENTED_EDGE('',*,*,#4265,.T.);
#6045=ORIENTED_EDGE('',*,*,#4266,.F.);
#6046=ORIENTED_EDGE('',*,*,#4267,.T.);
#6047=ORIENTED_EDGE('',*,*,#4263,.T.);
#6048=ORIENTED_EDGE('',*,*,#4268,.T.);
#6049=ORIENTED_EDGE('',*,*,#4269,.F.);
#6050=ORIENTED_EDGE('',*,*,#4270,.T.);
#6051=ORIENTED_EDGE('',*,*,#4266,.T.);
#6052=ORIENTED_EDGE('',*,*,#4271,.T.);
#6053=ORIENTED_EDGE('',*,*,#4272,.F.);
#6054=ORIENTED_EDGE('',*,*,#4273,.T.);
#6055=ORIENTED_EDGE('',*,*,#4269,.T.);
#6056=ORIENTED_EDGE('',*,*,#4274,.T.);
#6057=ORIENTED_EDGE('',*,*,#4275,.F.);
#6058=ORIENTED_EDGE('',*,*,#4276,.T.);
#6059=ORIENTED_EDGE('',*,*,#4272,.T.);
#6060=ORIENTED_EDGE('',*,*,#4277,.T.);
#6061=ORIENTED_EDGE('',*,*,#4278,.F.);
#6062=ORIENTED_EDGE('',*,*,#4279,.T.);
#6063=ORIENTED_EDGE('',*,*,#4275,.T.);
#6064=ORIENTED_EDGE('',*,*,#4280,.T.);
#6065=ORIENTED_EDGE('',*,*,#4281,.F.);
#6066=ORIENTED_EDGE('',*,*,#4282,.T.);
#6067=ORIENTED_EDGE('',*,*,#4278,.T.);
#6068=ORIENTED_EDGE('',*,*,#4283,.T.);
#6069=ORIENTED_EDGE('',*,*,#4284,.F.);
#6070=ORIENTED_EDGE('',*,*,#4285,.T.);
#6071=ORIENTED_EDGE('',*,*,#4281,.T.);
#6072=ORIENTED_EDGE('',*,*,#4286,.T.);
#6073=ORIENTED_EDGE('',*,*,#4287,.F.);
#6074=ORIENTED_EDGE('',*,*,#4288,.T.);
#6075=ORIENTED_EDGE('',*,*,#4284,.T.);
#6076=ORIENTED_EDGE('',*,*,#4289,.T.);
#6077=ORIENTED_EDGE('',*,*,#4290,.F.);
#6078=ORIENTED_EDGE('',*,*,#4291,.T.);
#6079=ORIENTED_EDGE('',*,*,#4287,.T.);
#6080=ORIENTED_EDGE('',*,*,#4292,.T.);
#6081=ORIENTED_EDGE('',*,*,#4293,.F.);
#6082=ORIENTED_EDGE('',*,*,#4294,.T.);
#6083=ORIENTED_EDGE('',*,*,#4290,.T.);
#6084=ORIENTED_EDGE('',*,*,#4295,.T.);
#6085=ORIENTED_EDGE('',*,*,#4296,.F.);
#6086=ORIENTED_EDGE('',*,*,#4297,.T.);
#6087=ORIENTED_EDGE('',*,*,#4293,.T.);
#6088=ORIENTED_EDGE('',*,*,#4298,.T.);
#6089=ORIENTED_EDGE('',*,*,#4299,.F.);
#6090=ORIENTED_EDGE('',*,*,#4300,.T.);
#6091=ORIENTED_EDGE('',*,*,#4296,.T.);
#6092=ORIENTED_EDGE('',*,*,#4301,.T.);
#6093=ORIENTED_EDGE('',*,*,#4302,.F.);
#6094=ORIENTED_EDGE('',*,*,#4303,.T.);
#6095=ORIENTED_EDGE('',*,*,#4299,.T.);
#6096=ORIENTED_EDGE('',*,*,#4304,.T.);
#6097=ORIENTED_EDGE('',*,*,#4305,.F.);
#6098=ORIENTED_EDGE('',*,*,#4306,.T.);
#6099=ORIENTED_EDGE('',*,*,#4302,.T.);
#6100=ORIENTED_EDGE('',*,*,#4307,.T.);
#6101=ORIENTED_EDGE('',*,*,#4308,.F.);
#6102=ORIENTED_EDGE('',*,*,#4309,.T.);
#6103=ORIENTED_EDGE('',*,*,#4305,.T.);
#6104=ORIENTED_EDGE('',*,*,#4310,.T.);
#6105=ORIENTED_EDGE('',*,*,#4311,.F.);
#6106=ORIENTED_EDGE('',*,*,#4312,.T.);
#6107=ORIENTED_EDGE('',*,*,#4308,.T.);
#6108=ORIENTED_EDGE('',*,*,#4313,.T.);
#6109=ORIENTED_EDGE('',*,*,#4314,.F.);
#6110=ORIENTED_EDGE('',*,*,#4315,.T.);
#6111=ORIENTED_EDGE('',*,*,#4311,.T.);
#6112=ORIENTED_EDGE('',*,*,#4316,.T.);
#6113=ORIENTED_EDGE('',*,*,#4317,.F.);
#6114=ORIENTED_EDGE('',*,*,#4318,.T.);
#6115=ORIENTED_EDGE('',*,*,#4314,.T.);
#6116=ORIENTED_EDGE('',*,*,#4319,.T.);
#6117=ORIENTED_EDGE('',*,*,#4320,.F.);
#6118=ORIENTED_EDGE('',*,*,#4321,.T.);
#6119=ORIENTED_EDGE('',*,*,#4317,.T.);
#6120=ORIENTED_EDGE('',*,*,#4322,.T.);
#6121=ORIENTED_EDGE('',*,*,#4323,.F.);
#6122=ORIENTED_EDGE('',*,*,#4324,.T.);
#6123=ORIENTED_EDGE('',*,*,#4320,.T.);
#6124=ORIENTED_EDGE('',*,*,#4325,.T.);
#6125=ORIENTED_EDGE('',*,*,#4326,.F.);
#6126=ORIENTED_EDGE('',*,*,#4327,.T.);
#6127=ORIENTED_EDGE('',*,*,#4323,.T.);
#6128=ORIENTED_EDGE('',*,*,#4328,.T.);
#6129=ORIENTED_EDGE('',*,*,#4329,.F.);
#6130=ORIENTED_EDGE('',*,*,#4330,.T.);
#6131=ORIENTED_EDGE('',*,*,#4326,.T.);
#6132=ORIENTED_EDGE('',*,*,#4331,.T.);
#6133=ORIENTED_EDGE('',*,*,#4332,.F.);
#6134=ORIENTED_EDGE('',*,*,#4333,.T.);
#6135=ORIENTED_EDGE('',*,*,#4329,.T.);
#6136=ORIENTED_EDGE('',*,*,#4334,.T.);
#6137=ORIENTED_EDGE('',*,*,#4335,.F.);
#6138=ORIENTED_EDGE('',*,*,#4336,.T.);
#6139=ORIENTED_EDGE('',*,*,#4332,.T.);
#6140=ORIENTED_EDGE('',*,*,#4337,.T.);
#6141=ORIENTED_EDGE('',*,*,#4338,.F.);
#6142=ORIENTED_EDGE('',*,*,#4339,.T.);
#6143=ORIENTED_EDGE('',*,*,#4335,.T.);
#6144=ORIENTED_EDGE('',*,*,#4340,.T.);
#6145=ORIENTED_EDGE('',*,*,#4341,.F.);
#6146=ORIENTED_EDGE('',*,*,#4342,.T.);
#6147=ORIENTED_EDGE('',*,*,#4338,.T.);
#6148=ORIENTED_EDGE('',*,*,#4343,.T.);
#6149=ORIENTED_EDGE('',*,*,#4344,.F.);
#6150=ORIENTED_EDGE('',*,*,#4345,.T.);
#6151=ORIENTED_EDGE('',*,*,#4341,.T.);
#6152=ORIENTED_EDGE('',*,*,#4346,.T.);
#6153=ORIENTED_EDGE('',*,*,#4347,.F.);
#6154=ORIENTED_EDGE('',*,*,#4348,.T.);
#6155=ORIENTED_EDGE('',*,*,#4344,.T.);
#6156=ORIENTED_EDGE('',*,*,#4349,.T.);
#6157=ORIENTED_EDGE('',*,*,#4350,.F.);
#6158=ORIENTED_EDGE('',*,*,#4351,.T.);
#6159=ORIENTED_EDGE('',*,*,#4352,.T.);
#6160=ORIENTED_EDGE('',*,*,#4353,.F.);
#6161=ORIENTED_EDGE('',*,*,#4354,.F.);
#6162=ORIENTED_EDGE('',*,*,#4355,.T.);
#6163=ORIENTED_EDGE('',*,*,#4350,.T.);
#6164=ORIENTED_EDGE('',*,*,#4356,.F.);
#6165=ORIENTED_EDGE('',*,*,#4357,.F.);
#6166=ORIENTED_EDGE('',*,*,#4358,.T.);
#6167=ORIENTED_EDGE('',*,*,#4354,.T.);
#6168=ORIENTED_EDGE('',*,*,#4359,.F.);
#6169=ORIENTED_EDGE('',*,*,#4360,.F.);
#6170=ORIENTED_EDGE('',*,*,#4361,.T.);
#6171=ORIENTED_EDGE('',*,*,#4357,.T.);
#6172=ORIENTED_EDGE('',*,*,#4362,.F.);
#6173=ORIENTED_EDGE('',*,*,#4363,.F.);
#6174=ORIENTED_EDGE('',*,*,#4364,.T.);
#6175=ORIENTED_EDGE('',*,*,#4360,.T.);
#6176=ORIENTED_EDGE('',*,*,#4365,.F.);
#6177=ORIENTED_EDGE('',*,*,#4366,.F.);
#6178=ORIENTED_EDGE('',*,*,#4367,.T.);
#6179=ORIENTED_EDGE('',*,*,#4363,.T.);
#6180=ORIENTED_EDGE('',*,*,#4368,.F.);
#6181=ORIENTED_EDGE('',*,*,#4369,.F.);
#6182=ORIENTED_EDGE('',*,*,#4370,.T.);
#6183=ORIENTED_EDGE('',*,*,#4366,.T.);
#6184=ORIENTED_EDGE('',*,*,#4371,.F.);
#6185=ORIENTED_EDGE('',*,*,#4372,.F.);
#6186=ORIENTED_EDGE('',*,*,#4373,.T.);
#6187=ORIENTED_EDGE('',*,*,#4369,.T.);
#6188=ORIENTED_EDGE('',*,*,#4374,.F.);
#6189=ORIENTED_EDGE('',*,*,#4375,.F.);
#6190=ORIENTED_EDGE('',*,*,#4376,.T.);
#6191=ORIENTED_EDGE('',*,*,#4372,.T.);
#6192=ORIENTED_EDGE('',*,*,#4377,.F.);
#6193=ORIENTED_EDGE('',*,*,#4378,.F.);
#6194=ORIENTED_EDGE('',*,*,#4379,.T.);
#6195=ORIENTED_EDGE('',*,*,#4375,.T.);
#6196=ORIENTED_EDGE('',*,*,#4380,.F.);
#6197=ORIENTED_EDGE('',*,*,#4381,.F.);
#6198=ORIENTED_EDGE('',*,*,#4382,.T.);
#6199=ORIENTED_EDGE('',*,*,#4378,.T.);
#6200=ORIENTED_EDGE('',*,*,#4383,.F.);
#6201=ORIENTED_EDGE('',*,*,#4384,.F.);
#6202=ORIENTED_EDGE('',*,*,#4385,.T.);
#6203=ORIENTED_EDGE('',*,*,#4381,.T.);
#6204=ORIENTED_EDGE('',*,*,#4386,.F.);
#6205=ORIENTED_EDGE('',*,*,#4387,.F.);
#6206=ORIENTED_EDGE('',*,*,#4388,.T.);
#6207=ORIENTED_EDGE('',*,*,#4384,.T.);
#6208=ORIENTED_EDGE('',*,*,#4389,.F.);
#6209=ORIENTED_EDGE('',*,*,#4390,.F.);
#6210=ORIENTED_EDGE('',*,*,#4391,.T.);
#6211=ORIENTED_EDGE('',*,*,#4387,.T.);
#6212=ORIENTED_EDGE('',*,*,#4392,.F.);
#6213=ORIENTED_EDGE('',*,*,#4393,.F.);
#6214=ORIENTED_EDGE('',*,*,#4394,.T.);
#6215=ORIENTED_EDGE('',*,*,#4390,.T.);
#6216=ORIENTED_EDGE('',*,*,#4395,.F.);
#6217=ORIENTED_EDGE('',*,*,#4396,.F.);
#6218=ORIENTED_EDGE('',*,*,#4397,.T.);
#6219=ORIENTED_EDGE('',*,*,#4393,.T.);
#6220=ORIENTED_EDGE('',*,*,#4398,.F.);
#6221=ORIENTED_EDGE('',*,*,#4399,.F.);
#6222=ORIENTED_EDGE('',*,*,#4400,.T.);
#6223=ORIENTED_EDGE('',*,*,#4396,.T.);
#6224=ORIENTED_EDGE('',*,*,#4401,.F.);
#6225=ORIENTED_EDGE('',*,*,#4402,.F.);
#6226=ORIENTED_EDGE('',*,*,#4403,.T.);
#6227=ORIENTED_EDGE('',*,*,#4399,.T.);
#6228=ORIENTED_EDGE('',*,*,#4404,.F.);
#6229=ORIENTED_EDGE('',*,*,#4405,.F.);
#6230=ORIENTED_EDGE('',*,*,#4406,.T.);
#6231=ORIENTED_EDGE('',*,*,#4402,.T.);
#6232=ORIENTED_EDGE('',*,*,#4407,.F.);
#6233=ORIENTED_EDGE('',*,*,#4408,.F.);
#6234=ORIENTED_EDGE('',*,*,#4409,.T.);
#6235=ORIENTED_EDGE('',*,*,#4405,.T.);
#6236=ORIENTED_EDGE('',*,*,#4410,.F.);
#6237=ORIENTED_EDGE('',*,*,#4411,.F.);
#6238=ORIENTED_EDGE('',*,*,#4412,.T.);
#6239=ORIENTED_EDGE('',*,*,#4408,.T.);
#6240=ORIENTED_EDGE('',*,*,#4413,.F.);
#6241=ORIENTED_EDGE('',*,*,#4414,.F.);
#6242=ORIENTED_EDGE('',*,*,#4415,.T.);
#6243=ORIENTED_EDGE('',*,*,#4411,.T.);
#6244=ORIENTED_EDGE('',*,*,#4416,.F.);
#6245=ORIENTED_EDGE('',*,*,#4417,.F.);
#6246=ORIENTED_EDGE('',*,*,#4418,.T.);
#6247=ORIENTED_EDGE('',*,*,#4414,.T.);
#6248=ORIENTED_EDGE('',*,*,#4419,.F.);
#6249=ORIENTED_EDGE('',*,*,#4420,.F.);
#6250=ORIENTED_EDGE('',*,*,#4421,.T.);
#6251=ORIENTED_EDGE('',*,*,#4417,.T.);
#6252=ORIENTED_EDGE('',*,*,#4422,.F.);
#6253=ORIENTED_EDGE('',*,*,#4423,.F.);
#6254=ORIENTED_EDGE('',*,*,#4424,.T.);
#6255=ORIENTED_EDGE('',*,*,#4420,.T.);
#6256=ORIENTED_EDGE('',*,*,#4425,.F.);
#6257=ORIENTED_EDGE('',*,*,#4426,.F.);
#6258=ORIENTED_EDGE('',*,*,#4427,.T.);
#6259=ORIENTED_EDGE('',*,*,#4423,.T.);
#6260=ORIENTED_EDGE('',*,*,#4428,.F.);
#6261=ORIENTED_EDGE('',*,*,#4429,.F.);
#6262=ORIENTED_EDGE('',*,*,#4430,.T.);
#6263=ORIENTED_EDGE('',*,*,#4426,.T.);
#6264=ORIENTED_EDGE('',*,*,#4431,.F.);
#6265=ORIENTED_EDGE('',*,*,#4432,.F.);
#6266=ORIENTED_EDGE('',*,*,#4433,.T.);
#6267=ORIENTED_EDGE('',*,*,#4429,.T.);
#6268=ORIENTED_EDGE('',*,*,#4434,.F.);
#6269=ORIENTED_EDGE('',*,*,#4435,.F.);
#6270=ORIENTED_EDGE('',*,*,#4436,.T.);
#6271=ORIENTED_EDGE('',*,*,#4432,.T.);
#6272=ORIENTED_EDGE('',*,*,#4437,.F.);
#6273=ORIENTED_EDGE('',*,*,#4438,.F.);
#6274=ORIENTED_EDGE('',*,*,#4439,.T.);
#6275=ORIENTED_EDGE('',*,*,#4435,.T.);
#6276=ORIENTED_EDGE('',*,*,#4440,.F.);
#6277=ORIENTED_EDGE('',*,*,#4441,.F.);
#6278=ORIENTED_EDGE('',*,*,#4352,.F.);
#6279=ORIENTED_EDGE('',*,*,#4442,.F.);
#6280=ORIENTED_EDGE('',*,*,#4443,.F.);
#6281=ORIENTED_EDGE('',*,*,#4444,.F.);
#6282=ORIENTED_EDGE('',*,*,#4445,.T.);
#6283=ORIENTED_EDGE('',*,*,#4446,.F.);
#6284=ORIENTED_EDGE('',*,*,#4445,.F.);
#6285=ORIENTED_EDGE('',*,*,#4442,.T.);
#6286=ORIENTED_EDGE('',*,*,#4351,.F.);
#6287=ORIENTED_EDGE('',*,*,#4355,.F.);
#6288=ORIENTED_EDGE('',*,*,#4358,.F.);
#6289=ORIENTED_EDGE('',*,*,#4361,.F.);
#6290=ORIENTED_EDGE('',*,*,#4364,.F.);
#6291=ORIENTED_EDGE('',*,*,#4367,.F.);
#6292=ORIENTED_EDGE('',*,*,#4370,.F.);
#6293=ORIENTED_EDGE('',*,*,#4373,.F.);
#6294=ORIENTED_EDGE('',*,*,#4376,.F.);
#6295=ORIENTED_EDGE('',*,*,#4379,.F.);
#6296=ORIENTED_EDGE('',*,*,#4382,.F.);
#6297=ORIENTED_EDGE('',*,*,#4385,.F.);
#6298=ORIENTED_EDGE('',*,*,#4388,.F.);
#6299=ORIENTED_EDGE('',*,*,#4391,.F.);
#6300=ORIENTED_EDGE('',*,*,#4394,.F.);
#6301=ORIENTED_EDGE('',*,*,#4397,.F.);
#6302=ORIENTED_EDGE('',*,*,#4400,.F.);
#6303=ORIENTED_EDGE('',*,*,#4403,.F.);
#6304=ORIENTED_EDGE('',*,*,#4406,.F.);
#6305=ORIENTED_EDGE('',*,*,#4409,.F.);
#6306=ORIENTED_EDGE('',*,*,#4412,.F.);
#6307=ORIENTED_EDGE('',*,*,#4415,.F.);
#6308=ORIENTED_EDGE('',*,*,#4418,.F.);
#6309=ORIENTED_EDGE('',*,*,#4421,.F.);
#6310=ORIENTED_EDGE('',*,*,#4424,.F.);
#6311=ORIENTED_EDGE('',*,*,#4427,.F.);
#6312=ORIENTED_EDGE('',*,*,#4430,.F.);
#6313=ORIENTED_EDGE('',*,*,#4433,.F.);
#6314=ORIENTED_EDGE('',*,*,#4436,.F.);
#6315=ORIENTED_EDGE('',*,*,#4439,.F.);
#6316=ORIENTED_EDGE('',*,*,#4447,.F.);
#6317=ORIENTED_EDGE('',*,*,#4448,.F.);
#6318=ORIENTED_EDGE('',*,*,#4260,.F.);
#6319=ORIENTED_EDGE('',*,*,#4264,.F.);
#6320=ORIENTED_EDGE('',*,*,#4267,.F.);
#6321=ORIENTED_EDGE('',*,*,#4270,.F.);
#6322=ORIENTED_EDGE('',*,*,#4273,.F.);
#6323=ORIENTED_EDGE('',*,*,#4276,.F.);
#6324=ORIENTED_EDGE('',*,*,#4279,.F.);
#6325=ORIENTED_EDGE('',*,*,#4282,.F.);
#6326=ORIENTED_EDGE('',*,*,#4285,.F.);
#6327=ORIENTED_EDGE('',*,*,#4288,.F.);
#6328=ORIENTED_EDGE('',*,*,#4291,.F.);
#6329=ORIENTED_EDGE('',*,*,#4294,.F.);
#6330=ORIENTED_EDGE('',*,*,#4297,.F.);
#6331=ORIENTED_EDGE('',*,*,#4300,.F.);
#6332=ORIENTED_EDGE('',*,*,#4303,.F.);
#6333=ORIENTED_EDGE('',*,*,#4306,.F.);
#6334=ORIENTED_EDGE('',*,*,#4309,.F.);
#6335=ORIENTED_EDGE('',*,*,#4312,.F.);
#6336=ORIENTED_EDGE('',*,*,#4315,.F.);
#6337=ORIENTED_EDGE('',*,*,#4318,.F.);
#6338=ORIENTED_EDGE('',*,*,#4321,.F.);
#6339=ORIENTED_EDGE('',*,*,#4324,.F.);
#6340=ORIENTED_EDGE('',*,*,#4327,.F.);
#6341=ORIENTED_EDGE('',*,*,#4330,.F.);
#6342=ORIENTED_EDGE('',*,*,#4333,.F.);
#6343=ORIENTED_EDGE('',*,*,#4336,.F.);
#6344=ORIENTED_EDGE('',*,*,#4339,.F.);
#6345=ORIENTED_EDGE('',*,*,#4342,.F.);
#6346=ORIENTED_EDGE('',*,*,#4345,.F.);
#6347=ORIENTED_EDGE('',*,*,#4348,.F.);
#6348=ORIENTED_EDGE('',*,*,#4449,.F.);
#6349=ORIENTED_EDGE('',*,*,#4438,.T.);
#6350=ORIENTED_EDGE('',*,*,#4450,.F.);
#6351=ORIENTED_EDGE('',*,*,#4451,.F.);
#6352=ORIENTED_EDGE('',*,*,#4447,.T.);
#6353=ORIENTED_EDGE('',*,*,#4441,.T.);
#6354=ORIENTED_EDGE('',*,*,#4444,.T.);
#6355=ORIENTED_EDGE('',*,*,#4452,.F.);
#6356=ORIENTED_EDGE('',*,*,#4349,.F.);
#6357=ORIENTED_EDGE('',*,*,#4346,.F.);
#6358=ORIENTED_EDGE('',*,*,#4343,.F.);
#6359=ORIENTED_EDGE('',*,*,#4340,.F.);
#6360=ORIENTED_EDGE('',*,*,#4337,.F.);
#6361=ORIENTED_EDGE('',*,*,#4334,.F.);
#6362=ORIENTED_EDGE('',*,*,#4331,.F.);
#6363=ORIENTED_EDGE('',*,*,#4328,.F.);
#6364=ORIENTED_EDGE('',*,*,#4325,.F.);
#6365=ORIENTED_EDGE('',*,*,#4322,.F.);
#6366=ORIENTED_EDGE('',*,*,#4319,.F.);
#6367=ORIENTED_EDGE('',*,*,#4316,.F.);
#6368=ORIENTED_EDGE('',*,*,#4313,.F.);
#6369=ORIENTED_EDGE('',*,*,#4310,.F.);
#6370=ORIENTED_EDGE('',*,*,#4307,.F.);
#6371=ORIENTED_EDGE('',*,*,#4304,.F.);
#6372=ORIENTED_EDGE('',*,*,#4301,.F.);
#6373=ORIENTED_EDGE('',*,*,#4298,.F.);
#6374=ORIENTED_EDGE('',*,*,#4295,.F.);
#6375=ORIENTED_EDGE('',*,*,#4292,.F.);
#6376=ORIENTED_EDGE('',*,*,#4289,.F.);
#6377=ORIENTED_EDGE('',*,*,#4286,.F.);
#6378=ORIENTED_EDGE('',*,*,#4283,.F.);
#6379=ORIENTED_EDGE('',*,*,#4280,.F.);
#6380=ORIENTED_EDGE('',*,*,#4277,.F.);
#6381=ORIENTED_EDGE('',*,*,#4274,.F.);
#6382=ORIENTED_EDGE('',*,*,#4271,.F.);
#6383=ORIENTED_EDGE('',*,*,#4268,.F.);
#6384=ORIENTED_EDGE('',*,*,#4265,.F.);
#6385=ORIENTED_EDGE('',*,*,#4262,.F.);
#6386=ORIENTED_EDGE('',*,*,#4453,.F.);
#6387=ORIENTED_EDGE('',*,*,#4450,.T.);
#6388=ORIENTED_EDGE('',*,*,#4440,.T.);
#6389=ORIENTED_EDGE('',*,*,#4437,.T.);
#6390=ORIENTED_EDGE('',*,*,#4434,.T.);
#6391=ORIENTED_EDGE('',*,*,#4431,.T.);
#6392=ORIENTED_EDGE('',*,*,#4428,.T.);
#6393=ORIENTED_EDGE('',*,*,#4425,.T.);
#6394=ORIENTED_EDGE('',*,*,#4422,.T.);
#6395=ORIENTED_EDGE('',*,*,#4419,.T.);
#6396=ORIENTED_EDGE('',*,*,#4416,.T.);
#6397=ORIENTED_EDGE('',*,*,#4413,.T.);
#6398=ORIENTED_EDGE('',*,*,#4410,.T.);
#6399=ORIENTED_EDGE('',*,*,#4407,.T.);
#6400=ORIENTED_EDGE('',*,*,#4404,.T.);
#6401=ORIENTED_EDGE('',*,*,#4401,.T.);
#6402=ORIENTED_EDGE('',*,*,#4398,.T.);
#6403=ORIENTED_EDGE('',*,*,#4395,.T.);
#6404=ORIENTED_EDGE('',*,*,#4392,.T.);
#6405=ORIENTED_EDGE('',*,*,#4389,.T.);
#6406=ORIENTED_EDGE('',*,*,#4386,.T.);
#6407=ORIENTED_EDGE('',*,*,#4383,.T.);
#6408=ORIENTED_EDGE('',*,*,#4380,.T.);
#6409=ORIENTED_EDGE('',*,*,#4377,.T.);
#6410=ORIENTED_EDGE('',*,*,#4374,.T.);
#6411=ORIENTED_EDGE('',*,*,#4371,.T.);
#6412=ORIENTED_EDGE('',*,*,#4368,.T.);
#6413=ORIENTED_EDGE('',*,*,#4365,.T.);
#6414=ORIENTED_EDGE('',*,*,#4362,.T.);
#6415=ORIENTED_EDGE('',*,*,#4359,.T.);
#6416=ORIENTED_EDGE('',*,*,#4356,.T.);
#6417=ORIENTED_EDGE('',*,*,#4353,.T.);
#6418=ORIENTED_EDGE('',*,*,#4347,.T.);
#6419=ORIENTED_EDGE('',*,*,#4452,.T.);
#6420=ORIENTED_EDGE('',*,*,#4443,.T.);
#6421=ORIENTED_EDGE('',*,*,#4449,.T.);
#6422=ORIENTED_EDGE('',*,*,#4454,.F.);
#6423=ORIENTED_EDGE('',*,*,#4455,.T.);
#6424=ORIENTED_EDGE('',*,*,#4456,.T.);
#6425=ORIENTED_EDGE('',*,*,#4457,.F.);
#6426=ORIENTED_EDGE('',*,*,#4458,.F.);
#6427=ORIENTED_EDGE('',*,*,#4459,.T.);
#6428=ORIENTED_EDGE('',*,*,#4460,.T.);
#6429=ORIENTED_EDGE('',*,*,#4455,.F.);
#6430=ORIENTED_EDGE('',*,*,#4461,.F.);
#6431=ORIENTED_EDGE('',*,*,#4462,.T.);
#6432=ORIENTED_EDGE('',*,*,#4463,.T.);
#6433=ORIENTED_EDGE('',*,*,#4459,.F.);
#6434=ORIENTED_EDGE('',*,*,#4464,.F.);
#6435=ORIENTED_EDGE('',*,*,#4465,.T.);
#6436=ORIENTED_EDGE('',*,*,#4466,.T.);
#6437=ORIENTED_EDGE('',*,*,#4462,.F.);
#6438=ORIENTED_EDGE('',*,*,#4467,.F.);
#6439=ORIENTED_EDGE('',*,*,#4468,.T.);
#6440=ORIENTED_EDGE('',*,*,#4469,.T.);
#6441=ORIENTED_EDGE('',*,*,#4465,.F.);
#6442=ORIENTED_EDGE('',*,*,#4470,.F.);
#6443=ORIENTED_EDGE('',*,*,#4457,.T.);
#6444=ORIENTED_EDGE('',*,*,#4471,.T.);
#6445=ORIENTED_EDGE('',*,*,#4468,.F.);
#6446=ORIENTED_EDGE('',*,*,#4471,.F.);
#6447=ORIENTED_EDGE('',*,*,#4456,.F.);
#6448=ORIENTED_EDGE('',*,*,#4460,.F.);
#6449=ORIENTED_EDGE('',*,*,#4463,.F.);
#6450=ORIENTED_EDGE('',*,*,#4466,.F.);
#6451=ORIENTED_EDGE('',*,*,#4469,.F.);
#6452=ORIENTED_EDGE('',*,*,#4472,.T.);
#6453=ORIENTED_EDGE('',*,*,#4448,.T.);
#6454=ORIENTED_EDGE('',*,*,#4451,.T.);
#6455=ORIENTED_EDGE('',*,*,#4453,.T.);
#6456=ORIENTED_EDGE('',*,*,#4261,.F.);
#6457=ORIENTED_EDGE('',*,*,#4472,.F.);
#6458=ORIENTED_EDGE('',*,*,#4473,.T.);
#6459=ORIENTED_EDGE('',*,*,#4474,.T.);
#6460=ORIENTED_EDGE('',*,*,#4473,.F.);
#6461=ORIENTED_EDGE('',*,*,#4474,.F.);
#6462=ORIENTED_EDGE('',*,*,#4454,.T.);
#6463=ORIENTED_EDGE('',*,*,#4470,.T.);
#6464=ORIENTED_EDGE('',*,*,#4467,.T.);
#6465=ORIENTED_EDGE('',*,*,#4464,.T.);
#6466=ORIENTED_EDGE('',*,*,#4461,.T.);
#6467=ORIENTED_EDGE('',*,*,#4458,.T.);
#6468=ORIENTED_EDGE('',*,*,#4446,.T.);
#6469=ORIENTED_EDGE('',*,*,#4475,.T.);
#6470=ORIENTED_EDGE('',*,*,#4476,.F.);
#6471=ORIENTED_EDGE('',*,*,#4477,.T.);
#6472=ORIENTED_EDGE('',*,*,#4478,.T.);
#6473=ORIENTED_EDGE('',*,*,#4479,.T.);
#6474=ORIENTED_EDGE('',*,*,#4480,.F.);
#6475=ORIENTED_EDGE('',*,*,#4475,.F.);
#6476=ORIENTED_EDGE('',*,*,#4481,.T.);
#6477=ORIENTED_EDGE('',*,*,#4482,.T.);
#6478=ORIENTED_EDGE('',*,*,#4483,.T.);
#6479=ORIENTED_EDGE('',*,*,#4478,.F.);
#6480=ORIENTED_EDGE('',*,*,#4484,.T.);
#6481=ORIENTED_EDGE('',*,*,#4485,.T.);
#6482=ORIENTED_EDGE('',*,*,#4486,.T.);
#6483=ORIENTED_EDGE('',*,*,#4482,.F.);
#6484=ORIENTED_EDGE('',*,*,#4487,.T.);
#6485=ORIENTED_EDGE('',*,*,#4488,.F.);
#6486=ORIENTED_EDGE('',*,*,#4489,.T.);
#6487=ORIENTED_EDGE('',*,*,#4490,.F.);
#6488=ORIENTED_EDGE('',*,*,#4491,.T.);
#6489=ORIENTED_EDGE('',*,*,#4492,.T.);
#6490=ORIENTED_EDGE('',*,*,#4493,.T.);
#6491=ORIENTED_EDGE('',*,*,#4494,.F.);
#6492=ORIENTED_EDGE('',*,*,#4495,.F.);
#6493=ORIENTED_EDGE('',*,*,#4496,.T.);
#6494=ORIENTED_EDGE('',*,*,#4497,.T.);
#6495=ORIENTED_EDGE('',*,*,#4492,.F.);
#6496=ORIENTED_EDGE('',*,*,#4498,.F.);
#6497=ORIENTED_EDGE('',*,*,#4499,.T.);
#6498=ORIENTED_EDGE('',*,*,#4500,.T.);
#6499=ORIENTED_EDGE('',*,*,#4496,.F.);
#6500=ORIENTED_EDGE('',*,*,#4501,.F.);
#6501=ORIENTED_EDGE('',*,*,#4502,.T.);
#6502=ORIENTED_EDGE('',*,*,#4503,.T.);
#6503=ORIENTED_EDGE('',*,*,#4499,.F.);
#6504=ORIENTED_EDGE('',*,*,#4504,.F.);
#6505=ORIENTED_EDGE('',*,*,#4505,.F.);
#6506=ORIENTED_EDGE('',*,*,#4506,.F.);
#6507=ORIENTED_EDGE('',*,*,#4507,.F.);
#6508=ORIENTED_EDGE('',*,*,#4508,.T.);
#6509=ORIENTED_EDGE('',*,*,#4505,.T.);
#6510=ORIENTED_EDGE('',*,*,#4509,.T.);
#6511=ORIENTED_EDGE('',*,*,#4502,.F.);
#6512=ORIENTED_EDGE('',*,*,#4510,.F.);
#6513=ORIENTED_EDGE('',*,*,#4511,.F.);
#6514=ORIENTED_EDGE('',*,*,#4493,.F.);
#6515=ORIENTED_EDGE('',*,*,#4497,.F.);
#6516=ORIENTED_EDGE('',*,*,#4500,.F.);
#6517=ORIENTED_EDGE('',*,*,#4503,.F.);
#6518=ORIENTED_EDGE('',*,*,#4509,.F.);
#6519=ORIENTED_EDGE('',*,*,#4508,.F.);
#6520=ORIENTED_EDGE('',*,*,#4512,.F.);
#6521=ORIENTED_EDGE('',*,*,#4489,.F.);
#6522=ORIENTED_EDGE('',*,*,#4513,.F.);
#6523=ORIENTED_EDGE('',*,*,#4487,.F.);
#6524=ORIENTED_EDGE('',*,*,#4484,.F.);
#6525=ORIENTED_EDGE('',*,*,#4481,.F.);
#6526=ORIENTED_EDGE('',*,*,#4477,.F.);
#6527=ORIENTED_EDGE('',*,*,#4514,.F.);
#6528=ORIENTED_EDGE('',*,*,#4479,.F.);
#6529=ORIENTED_EDGE('',*,*,#4483,.F.);
#6530=ORIENTED_EDGE('',*,*,#4486,.F.);
#6531=ORIENTED_EDGE('',*,*,#4515,.F.);
#6532=ORIENTED_EDGE('',*,*,#4491,.F.);
#6533=ORIENTED_EDGE('',*,*,#4516,.F.);
#6534=ORIENTED_EDGE('',*,*,#4506,.T.);
#6535=ORIENTED_EDGE('',*,*,#4510,.T.);
#6536=ORIENTED_EDGE('',*,*,#4504,.T.);
#6537=ORIENTED_EDGE('',*,*,#4501,.T.);
#6538=ORIENTED_EDGE('',*,*,#4498,.T.);
#6539=ORIENTED_EDGE('',*,*,#4495,.T.);
#6540=ORIENTED_EDGE('',*,*,#4517,.T.);
#6541=ORIENTED_EDGE('',*,*,#4518,.T.);
#6542=ORIENTED_EDGE('',*,*,#4519,.T.);
#6543=ORIENTED_EDGE('',*,*,#4520,.T.);
#6544=ORIENTED_EDGE('',*,*,#4521,.T.);
#6545=ORIENTED_EDGE('',*,*,#4522,.T.);
#6546=ORIENTED_EDGE('',*,*,#4512,.T.);
#6547=ORIENTED_EDGE('',*,*,#4507,.T.);
#6548=ORIENTED_EDGE('',*,*,#4516,.T.);
#6549=ORIENTED_EDGE('',*,*,#4490,.T.);
#6550=ORIENTED_EDGE('',*,*,#4488,.T.);
#6551=ORIENTED_EDGE('',*,*,#4515,.T.);
#6552=ORIENTED_EDGE('',*,*,#4485,.F.);
#6553=ORIENTED_EDGE('',*,*,#4513,.T.);
#6554=ORIENTED_EDGE('',*,*,#4523,.T.);
#6555=ORIENTED_EDGE('',*,*,#4524,.T.);
#6556=ORIENTED_EDGE('',*,*,#4522,.F.);
#6557=ORIENTED_EDGE('',*,*,#4525,.F.);
#6558=ORIENTED_EDGE('',*,*,#4526,.T.);
#6559=ORIENTED_EDGE('',*,*,#4525,.T.);
#6560=ORIENTED_EDGE('',*,*,#4521,.F.);
#6561=ORIENTED_EDGE('',*,*,#4527,.F.);
#6562=ORIENTED_EDGE('',*,*,#4528,.T.);
#6563=ORIENTED_EDGE('',*,*,#4527,.T.);
#6564=ORIENTED_EDGE('',*,*,#4520,.F.);
#6565=ORIENTED_EDGE('',*,*,#4529,.F.);
#6566=ORIENTED_EDGE('',*,*,#4530,.T.);
#6567=ORIENTED_EDGE('',*,*,#4529,.T.);
#6568=ORIENTED_EDGE('',*,*,#4519,.F.);
#6569=ORIENTED_EDGE('',*,*,#4531,.F.);
#6570=ORIENTED_EDGE('',*,*,#4532,.T.);
#6571=ORIENTED_EDGE('',*,*,#4531,.T.);
#6572=ORIENTED_EDGE('',*,*,#4518,.F.);
#6573=ORIENTED_EDGE('',*,*,#4533,.F.);
#6574=ORIENTED_EDGE('',*,*,#4534,.T.);
#6575=ORIENTED_EDGE('',*,*,#4533,.T.);
#6576=ORIENTED_EDGE('',*,*,#4517,.F.);
#6577=ORIENTED_EDGE('',*,*,#4524,.F.);
#6578=ORIENTED_EDGE('',*,*,#4534,.F.);
#6579=ORIENTED_EDGE('',*,*,#4523,.F.);
#6580=ORIENTED_EDGE('',*,*,#4526,.F.);
#6581=ORIENTED_EDGE('',*,*,#4528,.F.);
#6582=ORIENTED_EDGE('',*,*,#4530,.F.);
#6583=ORIENTED_EDGE('',*,*,#4532,.F.);
#6584=ORIENTED_EDGE('',*,*,#4511,.T.);
#6585=ORIENTED_EDGE('',*,*,#4476,.T.);
#6586=ORIENTED_EDGE('',*,*,#4480,.T.);
#6587=ORIENTED_EDGE('',*,*,#4514,.T.);
#6588=ORIENTED_EDGE('',*,*,#4494,.T.);
#6589=ORIENTED_EDGE('',*,*,#4535,.F.);
#6590=ORIENTED_EDGE('',*,*,#4536,.T.);
#6591=ORIENTED_EDGE('',*,*,#4537,.T.);
#6592=ORIENTED_EDGE('',*,*,#4536,.F.);
#6593=ORIENTED_EDGE('',*,*,#4538,.F.);
#6594=ORIENTED_EDGE('',*,*,#4539,.T.);
#6595=ORIENTED_EDGE('',*,*,#4540,.T.);
#6596=ORIENTED_EDGE('',*,*,#4539,.F.);
#6597=ORIENTED_EDGE('',*,*,#4538,.T.);
#6598=ORIENTED_EDGE('',*,*,#4535,.T.);
#6599=ORIENTED_EDGE('',*,*,#4540,.F.);
#6600=ORIENTED_EDGE('',*,*,#4537,.F.);
#6601=CYLINDRICAL_SURFACE('',#7274,0.17);
#6602=CYLINDRICAL_SURFACE('',#7277,0.17);
#6603=CYLINDRICAL_SURFACE('',#7280,0.41);
#6604=CYLINDRICAL_SURFACE('',#7289,0.2);
#6605=CYLINDRICAL_SURFACE('',#7292,17.7082646568653);
#6606=CYLINDRICAL_SURFACE('',#7307,1.4);
#6607=CYLINDRICAL_SURFACE('',#7309,1.4);
#6608=CYLINDRICAL_SURFACE('',#7318,1.1);
#6609=CYLINDRICAL_SURFACE('',#7323,1.7);
#6610=CYLINDRICAL_SURFACE('',#7324,1.7);
#6611=CYLINDRICAL_SURFACE('',#7334,0.17);
#6612=CYLINDRICAL_SURFACE('',#7337,0.17);
#6613=CYLINDRICAL_SURFACE('',#7340,0.41);
#6614=CYLINDRICAL_SURFACE('',#7351,0.2);
#6615=CYLINDRICAL_SURFACE('',#7353,17.7082646568653);
#6616=CYLINDRICAL_SURFACE('',#7367,1.4);
#6617=CYLINDRICAL_SURFACE('',#7369,1.4);
#6618=CYLINDRICAL_SURFACE('',#7378,1.1);
#6619=CYLINDRICAL_SURFACE('',#7383,1.7);
#6620=CYLINDRICAL_SURFACE('',#7384,1.7);
#6621=CYLINDRICAL_SURFACE('',#7394,0.3);
#6622=CYLINDRICAL_SURFACE('',#7401,0.4);
#6623=CYLINDRICAL_SURFACE('',#7406,0.6);
#6624=CYLINDRICAL_SURFACE('',#7409,0.4);
#6625=CYLINDRICAL_SURFACE('',#7417,0.3);
#6626=CYLINDRICAL_SURFACE('',#7419,0.6);
#6627=CYLINDRICAL_SURFACE('',#7424,0.15);
#6628=CYLINDRICAL_SURFACE('',#7427,0.15);
#6629=CYLINDRICAL_SURFACE('',#7430,0.15);
#6630=CYLINDRICAL_SURFACE('',#7433,0.15);
#6631=CYLINDRICAL_SURFACE('',#7436,0.3);
#6632=CYLINDRICAL_SURFACE('',#7441,0.3);
#6633=CYLINDRICAL_SURFACE('',#7446,0.17);
#6634=CYLINDRICAL_SURFACE('',#7448,0.17);
#6635=CYLINDRICAL_SURFACE('',#7472,0.4);
#6636=CYLINDRICAL_SURFACE('',#7474,0.4);
#6637=CYLINDRICAL_SURFACE('',#7498,0.1);
#6638=CYLINDRICAL_SURFACE('',#7502,0.1);
#6639=CYLINDRICAL_SURFACE('',#7516,0.3);
#6640=CYLINDRICAL_SURFACE('',#7521,0.3);
#6641=CYLINDRICAL_SURFACE('',#7526,0.15);
#6642=CYLINDRICAL_SURFACE('',#7529,0.15);
#6643=CYLINDRICAL_SURFACE('',#7532,0.15);
#6644=CYLINDRICAL_SURFACE('',#7535,0.15);
#6645=CYLINDRICAL_SURFACE('',#7554,0.17);
#6646=CYLINDRICAL_SURFACE('',#7556,0.17);
#6647=CYLINDRICAL_SURFACE('',#7580,0.4);
#6648=CYLINDRICAL_SURFACE('',#7582,0.4);
#6649=CYLINDRICAL_SURFACE('',#7606,0.1);
#6650=CYLINDRICAL_SURFACE('',#7610,0.1);
#6651=CYLINDRICAL_SURFACE('',#7624,0.3);
#6652=CYLINDRICAL_SURFACE('',#7629,0.3);
#6653=CYLINDRICAL_SURFACE('',#7634,0.35);
#6654=CYLINDRICAL_SURFACE('',#7637,0.35);
#6655=CYLINDRICAL_SURFACE('',#7643,0.25);
#6656=CYLINDRICAL_SURFACE('',#7649,0.25);
#6657=CYLINDRICAL_SURFACE('',#7655,0.25);
#6658=CYLINDRICAL_SURFACE('',#7661,0.25);
#6659=CYLINDRICAL_SURFACE('',#7664,0.15);
#6660=CYLINDRICAL_SURFACE('',#7666,0.15);
#6661=CYLINDRICAL_SURFACE('',#7668,0.15);
#6662=CYLINDRICAL_SURFACE('',#7670,0.15);
#6663=CYLINDRICAL_SURFACE('',#7674,0.08);
#6664=CYLINDRICAL_SURFACE('',#7679,0.08);
#6665=CYLINDRICAL_SURFACE('',#7687,0.14635);
#6666=CYLINDRICAL_SURFACE('',#7689,0.14635);
#6667=CYLINDRICAL_SURFACE('',#7690,0.14635);
#6668=CYLINDRICAL_SURFACE('',#7691,0.14635);
#6669=CYLINDRICAL_SURFACE('',#7692,0.14635);
#6670=CYLINDRICAL_SURFACE('',#7693,0.14635);
#6671=CYLINDRICAL_SURFACE('',#7694,0.14635);
#6672=CYLINDRICAL_SURFACE('',#7695,0.14635);
#6673=CYLINDRICAL_SURFACE('',#7696,0.14635);
#6674=CYLINDRICAL_SURFACE('',#7697,0.14635);
#6675=CYLINDRICAL_SURFACE('',#7698,0.14635);
#6676=CYLINDRICAL_SURFACE('',#7699,0.14635);
#6677=CYLINDRICAL_SURFACE('',#7700,0.14635);
#6678=CYLINDRICAL_SURFACE('',#7701,0.14635);
#6679=CYLINDRICAL_SURFACE('',#7702,0.14635);
#6680=CYLINDRICAL_SURFACE('',#7703,0.14635);
#6681=CYLINDRICAL_SURFACE('',#7704,0.14635);
#6682=CYLINDRICAL_SURFACE('',#7705,0.14635);
#6683=CYLINDRICAL_SURFACE('',#7706,0.14635);
#6684=CYLINDRICAL_SURFACE('',#7707,0.14635);
#6685=CYLINDRICAL_SURFACE('',#7708,0.14635);
#6686=CYLINDRICAL_SURFACE('',#7709,0.14635);
#6687=CYLINDRICAL_SURFACE('',#7710,0.14635);
#6688=CYLINDRICAL_SURFACE('',#7711,0.14635);
#6689=CYLINDRICAL_SURFACE('',#7712,0.14635);
#6690=CYLINDRICAL_SURFACE('',#7713,0.14635);
#6691=CYLINDRICAL_SURFACE('',#7714,0.14635);
#6692=CYLINDRICAL_SURFACE('',#7715,0.14635);
#6693=CYLINDRICAL_SURFACE('',#7716,0.14635);
#6694=CYLINDRICAL_SURFACE('',#7717,0.14635);
#6695=CYLINDRICAL_SURFACE('',#7718,0.117775);
#6696=CYLINDRICAL_SURFACE('',#7720,0.117775);
#6697=CYLINDRICAL_SURFACE('',#7721,0.117775);
#6698=CYLINDRICAL_SURFACE('',#7722,0.117775);
#6699=CYLINDRICAL_SURFACE('',#7723,0.117775);
#6700=CYLINDRICAL_SURFACE('',#7724,0.117775);
#6701=CYLINDRICAL_SURFACE('',#7725,0.117775);
#6702=CYLINDRICAL_SURFACE('',#7726,0.117775);
#6703=CYLINDRICAL_SURFACE('',#7727,0.117775);
#6704=CYLINDRICAL_SURFACE('',#7728,0.117775);
#6705=CYLINDRICAL_SURFACE('',#7729,0.117775);
#6706=CYLINDRICAL_SURFACE('',#7730,0.117775);
#6707=CYLINDRICAL_SURFACE('',#7731,0.117775);
#6708=CYLINDRICAL_SURFACE('',#7732,0.117775);
#6709=CYLINDRICAL_SURFACE('',#7733,0.117775);
#6710=CYLINDRICAL_SURFACE('',#7734,0.117775);
#6711=CYLINDRICAL_SURFACE('',#7735,0.117775);
#6712=CYLINDRICAL_SURFACE('',#7736,0.117775);
#6713=CYLINDRICAL_SURFACE('',#7737,0.117775);
#6714=CYLINDRICAL_SURFACE('',#7738,0.117775);
#6715=CYLINDRICAL_SURFACE('',#7739,0.117775);
#6716=CYLINDRICAL_SURFACE('',#7740,0.117775);
#6717=CYLINDRICAL_SURFACE('',#7741,0.117775);
#6718=CYLINDRICAL_SURFACE('',#7742,0.117775);
#6719=CYLINDRICAL_SURFACE('',#7743,0.117775);
#6720=CYLINDRICAL_SURFACE('',#7744,0.117775);
#6721=CYLINDRICAL_SURFACE('',#7745,0.117775);
#6722=CYLINDRICAL_SURFACE('',#7746,0.117775);
#6723=CYLINDRICAL_SURFACE('',#7747,0.117775);
#6724=CYLINDRICAL_SURFACE('',#7748,0.117775);
#6725=CYLINDRICAL_SURFACE('',#7752,0.117775);
#6726=CYLINDRICAL_SURFACE('',#7754,0.14635);
#6727=CYLINDRICAL_SURFACE('',#7764,0.275);
#6728=CYLINDRICAL_SURFACE('',#7769,0.12645);
#6729=CYLINDRICAL_SURFACE('',#7771,0.12645);
#6730=CYLINDRICAL_SURFACE('',#7773,0.12645);
#6731=CYLINDRICAL_SURFACE('',#7774,0.12645);
#6732=CYLINDRICAL_SURFACE('',#7775,0.12645);
#6733=CYLINDRICAL_SURFACE('',#7777,0.1543);
#6734=CYLINDRICAL_SURFACE('',#7779,0.1543);
#6735=CYLINDRICAL_SURFACE('',#7780,0.1543);
#6736=CYLINDRICAL_SURFACE('',#7781,0.1543);
#6737=CYLINDRICAL_SURFACE('',#7782,0.1543);
#6738=CYLINDRICAL_SURFACE('',#7784,0.1543);
#6739=CYLINDRICAL_SURFACE('',#7786,0.12645);
#6740=CYLINDRICAL_SURFACE('',#7803,0.41);
#6741=CYLINDRICAL_SURFACE('',#7806,0.6);
#6742=ADVANCED_FACE('',(#820),#6601,.F.);
#6743=ADVANCED_FACE('',(#821),#6602,.F.);
#6744=ADVANCED_FACE('',(#822),#6603,.F.);
#6745=ADVANCED_FACE('',(#823),#653,.F.);
#6746=ADVANCED_FACE('',(#824),#654,.F.);
#6747=ADVANCED_FACE('',(#825),#655,.T.);
#6748=ADVANCED_FACE('',(#826),#656,.T.);
#6749=ADVANCED_FACE('',(#827),#657,.T.);
#6750=ADVANCED_FACE('',(#828),#6604,.T.);
#6751=ADVANCED_FACE('',(#829),#6605,.T.);
#6752=ADVANCED_FACE('',(#830),#658,.F.);
#6753=ADVANCED_FACE('',(#831),#659,.T.);
#6754=ADVANCED_FACE('',(#832),#660,.T.);
#6755=ADVANCED_FACE('',(#833),#661,.T.);
#6756=ADVANCED_FACE('',(#834),#662,.T.);
#6757=ADVANCED_FACE('',(#835),#663,.T.);
#6758=ADVANCED_FACE('',(#836,#582,#583,#584,#585),#664,.F.);
#6759=ADVANCED_FACE('',(#837),#665,.T.);
#6760=ADVANCED_FACE('',(#838),#6606,.T.);
#6761=ADVANCED_FACE('',(#839),#6607,.T.);
#6762=ADVANCED_FACE('',(#840,#586,#587,#588,#589),#666,.T.);
#6763=ADVANCED_FACE('',(#841),#578,.T.);
#6764=ADVANCED_FACE('',(#842),#6608,.F.);
#6765=ADVANCED_FACE('',(#843),#579,.T.);
#6766=ADVANCED_FACE('',(#844),#6609,.T.);
#6767=ADVANCED_FACE('',(#845),#6610,.T.);
#6768=ADVANCED_FACE('',(#846),#667,.T.);
#6769=ADVANCED_FACE('',(#847),#668,.T.);
#6770=ADVANCED_FACE('',(#848),#669,.T.);
#6771=ADVANCED_FACE('',(#849),#670,.T.);
#6772=ADVANCED_FACE('',(#850),#671,.T.);
#6773=ADVANCED_FACE('',(#851),#672,.T.);
#6774=ADVANCED_FACE('',(#852),#673,.T.);
#6775=ADVANCED_FACE('',(#853),#674,.T.);
#6776=ADVANCED_FACE('',(#854),#6611,.F.);
#6777=ADVANCED_FACE('',(#855),#6612,.F.);
#6778=ADVANCED_FACE('',(#856),#6613,.F.);
#6779=ADVANCED_FACE('',(#857),#675,.F.);
#6780=ADVANCED_FACE('',(#858),#676,.F.);
#6781=ADVANCED_FACE('',(#859),#677,.T.);
#6782=ADVANCED_FACE('',(#860),#678,.T.);
#6783=ADVANCED_FACE('',(#861),#679,.T.);
#6784=ADVANCED_FACE('',(#862),#680,.T.);
#6785=ADVANCED_FACE('',(#863),#6614,.T.);
#6786=ADVANCED_FACE('',(#864),#6615,.T.);
#6787=ADVANCED_FACE('',(#865),#681,.F.);
#6788=ADVANCED_FACE('',(#866),#682,.T.);
#6789=ADVANCED_FACE('',(#867),#683,.T.);
#6790=ADVANCED_FACE('',(#868,#590,#591,#592,#593),#684,.F.);
#6791=ADVANCED_FACE('',(#869),#685,.T.);
#6792=ADVANCED_FACE('',(#870),#686,.T.);
#6793=ADVANCED_FACE('',(#871),#687,.T.);
#6794=ADVANCED_FACE('',(#872),#6616,.T.);
#6795=ADVANCED_FACE('',(#873),#6617,.T.);
#6796=ADVANCED_FACE('',(#874,#594,#595,#596,#597),#688,.T.);
#6797=ADVANCED_FACE('',(#875),#580,.T.);
#6798=ADVANCED_FACE('',(#876),#6618,.F.);
#6799=ADVANCED_FACE('',(#877),#581,.T.);
#6800=ADVANCED_FACE('',(#878),#6619,.T.);
#6801=ADVANCED_FACE('',(#879),#6620,.T.);
#6802=ADVANCED_FACE('',(#880),#689,.T.);
#6803=ADVANCED_FACE('',(#881),#690,.T.);
#6804=ADVANCED_FACE('',(#882),#691,.T.);
#6805=ADVANCED_FACE('',(#883),#692,.T.);
#6806=ADVANCED_FACE('',(#884),#693,.T.);
#6807=ADVANCED_FACE('',(#885),#694,.T.);
#6808=ADVANCED_FACE('',(#886),#695,.T.);
#6809=ADVANCED_FACE('',(#887),#696,.T.);
#6810=ADVANCED_FACE('',(#888),#6621,.T.);
#6811=ADVANCED_FACE('',(#889,#598),#697,.F.);
#6812=ADVANCED_FACE('',(#890,#599),#698,.F.);
#6813=ADVANCED_FACE('',(#891),#6622,.T.);
#6814=ADVANCED_FACE('',(#892,#600),#699,.T.);
#6815=ADVANCED_FACE('',(#893),#6623,.T.);
#6816=ADVANCED_FACE('',(#894),#700,.F.);
#6817=ADVANCED_FACE('',(#895),#6624,.T.);
#6818=ADVANCED_FACE('',(#896),#701,.T.);
#6819=ADVANCED_FACE('',(#897),#702,.F.);
#6820=ADVANCED_FACE('',(#898),#703,.F.);
#6821=ADVANCED_FACE('',(#899),#704,.F.);
#6822=ADVANCED_FACE('',(#900),#6625,.F.);
#6823=ADVANCED_FACE('',(#901),#6626,.T.);
#6824=ADVANCED_FACE('',(#902),#705,.T.);
#6825=ADVANCED_FACE('',(#903),#6627,.F.);
#6826=ADVANCED_FACE('',(#904),#6628,.F.);
#6827=ADVANCED_FACE('',(#905),#6629,.F.);
#6828=ADVANCED_FACE('',(#906),#6630,.F.);
#6829=ADVANCED_FACE('',(#907),#6631,.F.);
#6830=ADVANCED_FACE('',(#908,#601),#706,.F.);
#6831=ADVANCED_FACE('',(#909),#6632,.F.);
#6832=ADVANCED_FACE('',(#910,#602),#707,.F.);
#6833=ADVANCED_FACE('',(#911),#6633,.F.);
#6834=ADVANCED_FACE('',(#912),#6634,.F.);
#6835=ADVANCED_FACE('',(#913),#708,.F.);
#6836=ADVANCED_FACE('',(#914),#709,.F.);
#6837=ADVANCED_FACE('',(#915),#710,.F.);
#6838=ADVANCED_FACE('',(#916),#711,.F.);
#6839=ADVANCED_FACE('',(#917),#712,.F.);
#6840=ADVANCED_FACE('',(#918),#713,.F.);
#6841=ADVANCED_FACE('',(#919),#714,.F.);
#6842=ADVANCED_FACE('',(#920,#603),#715,.F.);
#6843=ADVANCED_FACE('',(#921,#604),#716,.F.);
#6844=ADVANCED_FACE('',(#922),#717,.F.);
#6845=ADVANCED_FACE('',(#923),#718,.F.);
#6846=ADVANCED_FACE('',(#924),#719,.F.);
#6847=ADVANCED_FACE('',(#925),#720,.F.);
#6848=ADVANCED_FACE('',(#926),#721,.F.);
#6849=ADVANCED_FACE('',(#927),#722,.T.);
#6850=ADVANCED_FACE('',(#928),#723,.T.);
#6851=ADVANCED_FACE('',(#929),#724,.T.);
#6852=ADVANCED_FACE('',(#930),#725,.T.);
#6853=ADVANCED_FACE('',(#931),#726,.T.);
#6854=ADVANCED_FACE('',(#932,#605),#727,.F.);
#6855=ADVANCED_FACE('',(#933),#6635,.T.);
#6856=ADVANCED_FACE('',(#934),#6636,.T.);
#6857=ADVANCED_FACE('',(#935),#728,.T.);
#6858=ADVANCED_FACE('',(#936),#92,.T.);
#6859=ADVANCED_FACE('',(#937),#93,.T.);
#6860=ADVANCED_FACE('',(#938),#94,.T.);
#6861=ADVANCED_FACE('',(#939),#95,.T.);
#6862=ADVANCED_FACE('',(#940,#606,#607,#608),#729,.F.);
#6863=ADVANCED_FACE('',(#941),#730,.F.);
#6864=ADVANCED_FACE('',(#942),#96,.T.);
#6865=ADVANCED_FACE('',(#943),#97,.T.);
#6866=ADVANCED_FACE('',(#944),#98,.T.);
#6867=ADVANCED_FACE('',(#945),#731,.T.);
#6868=ADVANCED_FACE('',(#946),#99,.T.);
#6869=ADVANCED_FACE('',(#947),#100,.T.);
#6870=ADVANCED_FACE('',(#948),#732,.F.);
#6871=ADVANCED_FACE('',(#949),#101,.T.);
#6872=ADVANCED_FACE('',(#950),#102,.T.);
#6873=ADVANCED_FACE('',(#951),#733,.T.);
#6874=ADVANCED_FACE('',(#952),#103,.T.);
#6875=ADVANCED_FACE('',(#953),#104,.T.);
#6876=ADVANCED_FACE('',(#954,#609,#610,#611),#734,.F.);
#6877=ADVANCED_FACE('',(#955),#105,.T.);
#6878=ADVANCED_FACE('',(#956),#106,.T.);
#6879=ADVANCED_FACE('',(#957),#735,.T.);
#6880=ADVANCED_FACE('',(#958),#107,.T.);
#6881=ADVANCED_FACE('',(#959),#108,.T.);
#6882=ADVANCED_FACE('',(#960),#736,.F.);
#6883=ADVANCED_FACE('',(#961),#109,.T.);
#6884=ADVANCED_FACE('',(#962),#110,.T.);
#6885=ADVANCED_FACE('',(#963),#76,.F.);
#6886=ADVANCED_FACE('',(#964),#77,.F.);
#6887=ADVANCED_FACE('',(#965),#78,.F.);
#6888=ADVANCED_FACE('',(#966),#6637,.F.);
#6889=ADVANCED_FACE('',(#967),#111,.T.);
#6890=ADVANCED_FACE('',(#968),#79,.F.);
#6891=ADVANCED_FACE('',(#969),#6638,.F.);
#6892=ADVANCED_FACE('',(#970),#112,.T.);
#6893=ADVANCED_FACE('',(#971),#113,.T.);
#6894=ADVANCED_FACE('',(#972),#114,.T.);
#6895=ADVANCED_FACE('',(#973),#115,.T.);
#6896=ADVANCED_FACE('',(#974),#737,.T.);
#6897=ADVANCED_FACE('',(#975),#80,.T.);
#6898=ADVANCED_FACE('',(#976),#81,.T.);
#6899=ADVANCED_FACE('',(#977),#82,.T.);
#6900=ADVANCED_FACE('',(#978),#6639,.T.);
#6901=ADVANCED_FACE('',(#979),#116,.F.);
#6902=ADVANCED_FACE('',(#980),#83,.T.);
#6903=ADVANCED_FACE('',(#981),#6640,.T.);
#6904=ADVANCED_FACE('',(#982),#117,.F.);
#6905=ADVANCED_FACE('',(#983),#118,.F.);
#6906=ADVANCED_FACE('',(#984),#119,.F.);
#6907=ADVANCED_FACE('',(#985),#120,.F.);
#6908=ADVANCED_FACE('',(#986),#121,.F.);
#6909=ADVANCED_FACE('',(#987),#122,.F.);
#6910=ADVANCED_FACE('',(#988),#738,.F.);
#6911=ADVANCED_FACE('',(#989,#612,#613,#614,#615,#616,#617),#739,.T.);
#6912=ADVANCED_FACE('',(#990),#123,.F.);
#6913=ADVANCED_FACE('',(#991),#740,.F.);
#6914=ADVANCED_FACE('',(#992),#6641,.F.);
#6915=ADVANCED_FACE('',(#993),#6642,.F.);
#6916=ADVANCED_FACE('',(#994),#6643,.F.);
#6917=ADVANCED_FACE('',(#995),#6644,.F.);
#6918=ADVANCED_FACE('',(#996),#741,.F.);
#6919=ADVANCED_FACE('',(#997),#742,.F.);
#6920=ADVANCED_FACE('',(#998),#743,.F.);
#6921=ADVANCED_FACE('',(#999),#744,.F.);
#6922=ADVANCED_FACE('',(#1000),#745,.F.);
#6923=ADVANCED_FACE('',(#1001),#746,.F.);
#6924=ADVANCED_FACE('',(#1002,#618),#747,.F.);
#6925=ADVANCED_FACE('',(#1003),#748,.F.);
#6926=ADVANCED_FACE('',(#1004),#749,.F.);
#6927=ADVANCED_FACE('',(#1005),#750,.F.);
#6928=ADVANCED_FACE('',(#1006),#751,.F.);
#6929=ADVANCED_FACE('',(#1007),#752,.F.);
#6930=ADVANCED_FACE('',(#1008),#753,.F.);
#6931=ADVANCED_FACE('',(#1009,#619),#754,.F.);
#6932=ADVANCED_FACE('',(#1010),#6645,.F.);
#6933=ADVANCED_FACE('',(#1011),#6646,.F.);
#6934=ADVANCED_FACE('',(#1012),#755,.F.);
#6935=ADVANCED_FACE('',(#1013),#756,.F.);
#6936=ADVANCED_FACE('',(#1014),#757,.F.);
#6937=ADVANCED_FACE('',(#1015),#758,.F.);
#6938=ADVANCED_FACE('',(#1016),#759,.F.);
#6939=ADVANCED_FACE('',(#1017),#760,.F.);
#6940=ADVANCED_FACE('',(#1018),#761,.F.);
#6941=ADVANCED_FACE('',(#1019,#620),#762,.F.);
#6942=ADVANCED_FACE('',(#1020,#621),#763,.F.);
#6943=ADVANCED_FACE('',(#1021),#764,.F.);
#6944=ADVANCED_FACE('',(#1022),#765,.F.);
#6945=ADVANCED_FACE('',(#1023),#766,.F.);
#6946=ADVANCED_FACE('',(#1024),#767,.F.);
#6947=ADVANCED_FACE('',(#1025),#768,.F.);
#6948=ADVANCED_FACE('',(#1026),#769,.T.);
#6949=ADVANCED_FACE('',(#1027),#770,.T.);
#6950=ADVANCED_FACE('',(#1028),#771,.T.);
#6951=ADVANCED_FACE('',(#1029),#772,.T.);
#6952=ADVANCED_FACE('',(#1030),#773,.T.);
#6953=ADVANCED_FACE('',(#1031,#622),#774,.F.);
#6954=ADVANCED_FACE('',(#1032),#6647,.T.);
#6955=ADVANCED_FACE('',(#1033),#6648,.T.);
#6956=ADVANCED_FACE('',(#1034),#775,.T.);
#6957=ADVANCED_FACE('',(#1035),#124,.T.);
#6958=ADVANCED_FACE('',(#1036),#125,.T.);
#6959=ADVANCED_FACE('',(#1037),#126,.T.);
#6960=ADVANCED_FACE('',(#1038),#127,.T.);
#6961=ADVANCED_FACE('',(#1039,#623,#624,#625),#776,.F.);
#6962=ADVANCED_FACE('',(#1040),#777,.F.);
#6963=ADVANCED_FACE('',(#1041),#128,.T.);
#6964=ADVANCED_FACE('',(#1042),#129,.T.);
#6965=ADVANCED_FACE('',(#1043),#130,.T.);
#6966=ADVANCED_FACE('',(#1044),#778,.T.);
#6967=ADVANCED_FACE('',(#1045),#131,.T.);
#6968=ADVANCED_FACE('',(#1046),#132,.T.);
#6969=ADVANCED_FACE('',(#1047),#779,.F.);
#6970=ADVANCED_FACE('',(#1048),#133,.T.);
#6971=ADVANCED_FACE('',(#1049),#134,.T.);
#6972=ADVANCED_FACE('',(#1050),#780,.T.);
#6973=ADVANCED_FACE('',(#1051),#135,.T.);
#6974=ADVANCED_FACE('',(#1052),#136,.T.);
#6975=ADVANCED_FACE('',(#1053,#626,#627,#628),#781,.F.);
#6976=ADVANCED_FACE('',(#1054),#137,.T.);
#6977=ADVANCED_FACE('',(#1055),#138,.T.);
#6978=ADVANCED_FACE('',(#1056),#782,.T.);
#6979=ADVANCED_FACE('',(#1057),#139,.T.);
#6980=ADVANCED_FACE('',(#1058),#140,.T.);
#6981=ADVANCED_FACE('',(#1059),#783,.F.);
#6982=ADVANCED_FACE('',(#1060),#141,.T.);
#6983=ADVANCED_FACE('',(#1061),#142,.T.);
#6984=ADVANCED_FACE('',(#1062),#84,.F.);
#6985=ADVANCED_FACE('',(#1063),#85,.F.);
#6986=ADVANCED_FACE('',(#1064),#86,.F.);
#6987=ADVANCED_FACE('',(#1065),#6649,.F.);
#6988=ADVANCED_FACE('',(#1066),#143,.T.);
#6989=ADVANCED_FACE('',(#1067),#87,.F.);
#6990=ADVANCED_FACE('',(#1068),#6650,.F.);
#6991=ADVANCED_FACE('',(#1069),#144,.T.);
#6992=ADVANCED_FACE('',(#1070),#145,.T.);
#6993=ADVANCED_FACE('',(#1071),#146,.T.);
#6994=ADVANCED_FACE('',(#1072),#147,.T.);
#6995=ADVANCED_FACE('',(#1073),#784,.T.);
#6996=ADVANCED_FACE('',(#1074),#88,.T.);
#6997=ADVANCED_FACE('',(#1075),#89,.T.);
#6998=ADVANCED_FACE('',(#1076),#90,.T.);
#6999=ADVANCED_FACE('',(#1077),#6651,.T.);
#7000=ADVANCED_FACE('',(#1078),#148,.F.);
#7001=ADVANCED_FACE('',(#1079),#91,.T.);
#7002=ADVANCED_FACE('',(#1080),#6652,.T.);
#7003=ADVANCED_FACE('',(#1081),#149,.F.);
#7004=ADVANCED_FACE('',(#1082),#150,.F.);
#7005=ADVANCED_FACE('',(#1083),#151,.F.);
#7006=ADVANCED_FACE('',(#1084),#152,.F.);
#7007=ADVANCED_FACE('',(#1085),#153,.F.);
#7008=ADVANCED_FACE('',(#1086),#154,.F.);
#7009=ADVANCED_FACE('',(#1087),#785,.F.);
#7010=ADVANCED_FACE('',(#1088,#629,#630,#631,#632,#633,#634),#786,.T.);
#7011=ADVANCED_FACE('',(#1089),#155,.F.);
#7012=ADVANCED_FACE('',(#1090),#787,.F.);
#7013=ADVANCED_FACE('',(#1091),#6653,.F.);
#7014=ADVANCED_FACE('',(#1092),#6654,.F.);
#7015=ADVANCED_FACE('',(#1093,#635),#788,.T.);
#7016=ADVANCED_FACE('',(#1094),#6655,.T.);
#7017=ADVANCED_FACE('',(#1095),#789,.F.);
#7018=ADVANCED_FACE('',(#1096,#636),#790,.T.);
#7019=ADVANCED_FACE('',(#1097),#6656,.T.);
#7020=ADVANCED_FACE('',(#1098),#791,.F.);
#7021=ADVANCED_FACE('',(#1099,#637),#792,.T.);
#7022=ADVANCED_FACE('',(#1100),#6657,.T.);
#7023=ADVANCED_FACE('',(#1101),#793,.F.);
#7024=ADVANCED_FACE('',(#1102,#638),#794,.T.);
#7025=ADVANCED_FACE('',(#1103),#6658,.T.);
#7026=ADVANCED_FACE('',(#1104),#795,.F.);
#7027=ADVANCED_FACE('',(#1105),#6659,.T.);
#7028=ADVANCED_FACE('',(#1106),#6660,.T.);
#7029=ADVANCED_FACE('',(#1107),#6661,.T.);
#7030=ADVANCED_FACE('',(#1108),#6662,.T.);
#7031=ADVANCED_FACE('',(#1109),#156,.F.);
#7032=ADVANCED_FACE('',(#1110),#6663,.T.);
#7033=ADVANCED_FACE('',(#1111),#157,.F.);
#7034=ADVANCED_FACE('',(#1112),#158,.F.);
#7035=ADVANCED_FACE('',(#1113),#159,.F.);
#7036=ADVANCED_FACE('',(#1114),#6664,.T.);
#7037=ADVANCED_FACE('',(#1115),#160,.F.);
#7038=ADVANCED_FACE('',(#1116),#161,.F.);
#7039=ADVANCED_FACE('',(#1117),#796,.F.);
#7040=ADVANCED_FACE('',(#1118),#162,.F.);
#7041=ADVANCED_FACE('',(#1119),#163,.F.);
#7042=ADVANCED_FACE('',(#1120),#164,.F.);
#7043=ADVANCED_FACE('',(#1121,#639,#640),#797,.T.);
#7044=ADVANCED_FACE('',(#1122),#798,.F.);
#7045=ADVANCED_FACE('',(#1123),#165,.F.);
#7046=ADVANCED_FACE('',(#1124),#166,.F.);
#7047=ADVANCED_FACE('',(#1125,#641,#642,#643,#644,#645,#646),#799,.F.);
#7048=ADVANCED_FACE('',(#1126),#167,.F.);
#7049=ADVANCED_FACE('',(#1127),#6665,.T.);
#7050=ADVANCED_FACE('',(#1128),#6666,.T.);
#7051=ADVANCED_FACE('',(#1129),#6667,.T.);
#7052=ADVANCED_FACE('',(#1130),#6668,.T.);
#7053=ADVANCED_FACE('',(#1131),#6669,.T.);
#7054=ADVANCED_FACE('',(#1132),#6670,.T.);
#7055=ADVANCED_FACE('',(#1133),#6671,.T.);
#7056=ADVANCED_FACE('',(#1134),#6672,.T.);
#7057=ADVANCED_FACE('',(#1135),#6673,.T.);
#7058=ADVANCED_FACE('',(#1136),#6674,.T.);
#7059=ADVANCED_FACE('',(#1137),#6675,.T.);
#7060=ADVANCED_FACE('',(#1138),#6676,.T.);
#7061=ADVANCED_FACE('',(#1139),#6677,.T.);
#7062=ADVANCED_FACE('',(#1140),#6678,.T.);
#7063=ADVANCED_FACE('',(#1141),#6679,.T.);
#7064=ADVANCED_FACE('',(#1142),#6680,.T.);
#7065=ADVANCED_FACE('',(#1143),#6681,.T.);
#7066=ADVANCED_FACE('',(#1144),#6682,.T.);
#7067=ADVANCED_FACE('',(#1145),#6683,.T.);
#7068=ADVANCED_FACE('',(#1146),#6684,.T.);
#7069=ADVANCED_FACE('',(#1147),#6685,.T.);
#7070=ADVANCED_FACE('',(#1148),#6686,.T.);
#7071=ADVANCED_FACE('',(#1149),#6687,.T.);
#7072=ADVANCED_FACE('',(#1150),#6688,.T.);
#7073=ADVANCED_FACE('',(#1151),#6689,.T.);
#7074=ADVANCED_FACE('',(#1152),#6690,.T.);
#7075=ADVANCED_FACE('',(#1153),#6691,.T.);
#7076=ADVANCED_FACE('',(#1154),#6692,.T.);
#7077=ADVANCED_FACE('',(#1155),#6693,.T.);
#7078=ADVANCED_FACE('',(#1156),#6694,.T.);
#7079=ADVANCED_FACE('',(#1157),#6695,.T.);
#7080=ADVANCED_FACE('',(#1158),#6696,.T.);
#7081=ADVANCED_FACE('',(#1159),#6697,.T.);
#7082=ADVANCED_FACE('',(#1160),#6698,.T.);
#7083=ADVANCED_FACE('',(#1161),#6699,.T.);
#7084=ADVANCED_FACE('',(#1162),#6700,.T.);
#7085=ADVANCED_FACE('',(#1163),#6701,.T.);
#7086=ADVANCED_FACE('',(#1164),#6702,.T.);
#7087=ADVANCED_FACE('',(#1165),#6703,.T.);
#7088=ADVANCED_FACE('',(#1166),#6704,.T.);
#7089=ADVANCED_FACE('',(#1167),#6705,.T.);
#7090=ADVANCED_FACE('',(#1168),#6706,.T.);
#7091=ADVANCED_FACE('',(#1169),#6707,.T.);
#7092=ADVANCED_FACE('',(#1170),#6708,.T.);
#7093=ADVANCED_FACE('',(#1171),#6709,.T.);
#7094=ADVANCED_FACE('',(#1172),#6710,.T.);
#7095=ADVANCED_FACE('',(#1173),#6711,.T.);
#7096=ADVANCED_FACE('',(#1174),#6712,.T.);
#7097=ADVANCED_FACE('',(#1175),#6713,.T.);
#7098=ADVANCED_FACE('',(#1176),#6714,.T.);
#7099=ADVANCED_FACE('',(#1177),#6715,.T.);
#7100=ADVANCED_FACE('',(#1178),#6716,.T.);
#7101=ADVANCED_FACE('',(#1179),#6717,.T.);
#7102=ADVANCED_FACE('',(#1180),#6718,.T.);
#7103=ADVANCED_FACE('',(#1181),#6719,.T.);
#7104=ADVANCED_FACE('',(#1182),#6720,.T.);
#7105=ADVANCED_FACE('',(#1183),#6721,.T.);
#7106=ADVANCED_FACE('',(#1184),#6722,.T.);
#7107=ADVANCED_FACE('',(#1185),#6723,.T.);
#7108=ADVANCED_FACE('',(#1186),#6724,.T.);
#7109=ADVANCED_FACE('',(#1187),#75,.T.);
#7110=ADVANCED_FACE('',(#1188),#168,.F.);
#7111=ADVANCED_FACE('',(#1189),#6725,.T.);
#7112=ADVANCED_FACE('',(#1190),#169,.F.);
#7113=ADVANCED_FACE('',(#1191),#6726,.T.);
#7114=ADVANCED_FACE('',(#1192),#800,.F.);
#7115=ADVANCED_FACE('',(#1193),#801,.F.);
#7116=ADVANCED_FACE('',(#1194),#802,.F.);
#7117=ADVANCED_FACE('',(#1195),#803,.F.);
#7118=ADVANCED_FACE('',(#1196),#804,.F.);
#7119=ADVANCED_FACE('',(#1197),#805,.F.);
#7120=ADVANCED_FACE('',(#1198),#806,.F.);
#7121=ADVANCED_FACE('',(#1199,#647),#807,.T.);
#7122=ADVANCED_FACE('',(#1200),#6727,.T.);
#7123=ADVANCED_FACE('',(#1201,#648),#808,.F.);
#7124=ADVANCED_FACE('',(#1202),#809,.T.);
#7125=ADVANCED_FACE('',(#1203),#6728,.F.);
#7126=ADVANCED_FACE('',(#1204),#6729,.F.);
#7127=ADVANCED_FACE('',(#1205),#6730,.F.);
#7128=ADVANCED_FACE('',(#1206),#6731,.F.);
#7129=ADVANCED_FACE('',(#1207),#6732,.F.);
#7130=ADVANCED_FACE('',(#1208),#6733,.F.);
#7131=ADVANCED_FACE('',(#1209),#6734,.F.);
#7132=ADVANCED_FACE('',(#1210),#6735,.F.);
#7133=ADVANCED_FACE('',(#1211),#6736,.F.);
#7134=ADVANCED_FACE('',(#1212),#6737,.F.);
#7135=ADVANCED_FACE('',(#1213),#6738,.F.);
#7136=ADVANCED_FACE('',(#1214),#170,.F.);
#7137=ADVANCED_FACE('',(#1215),#171,.F.);
#7138=ADVANCED_FACE('',(#1216,#649),#810,.T.);
#7139=ADVANCED_FACE('',(#1217),#6739,.F.);
#7140=ADVANCED_FACE('',(#1218),#811,.T.);
#7141=ADVANCED_FACE('',(#1219),#812,.T.);
#7142=ADVANCED_FACE('',(#1220),#813,.T.);
#7143=ADVANCED_FACE('',(#1221),#814,.T.);
#7144=ADVANCED_FACE('',(#1222),#815,.T.);
#7145=ADVANCED_FACE('',(#1223),#816,.T.);
#7146=ADVANCED_FACE('',(#1224,#650),#817,.F.);
#7147=ADVANCED_FACE('',(#1225),#6740,.F.);
#7148=ADVANCED_FACE('',(#1226),#6741,.T.);
#7149=ADVANCED_FACE('',(#1227,#651),#818,.T.);
#7150=ADVANCED_FACE('',(#1228,#652),#819,.F.);
#7151=CLOSED_SHELL('',(#6742,#6743,#6744,#6745,#6746,#6747,#6748,#6749,
#6750,#6751,#6752,#6753,#6754,#6755,#6756,#6757,#6758,#6759,#6760,#6761,
#6762,#6763,#6764,#6765,#6766,#6767,#6768,#6769,#6770,#6771,#6772,#6773,
#6774,#6775));
#7152=CLOSED_SHELL('',(#6776,#6777,#6778,#6779,#6780,#6781,#6782,#6783,
#6784,#6785,#6786,#6787,#6788,#6789,#6790,#6791,#6792,#6793,#6794,#6795,
#6796,#6797,#6798,#6799,#6800,#6801,#6802,#6803,#6804,#6805,#6806,#6807,
#6808,#6809));
#7153=CLOSED_SHELL('',(#6810,#6811,#6812,#6813,#6814,#6815,#6816,#6817,
#6818));
#7154=CLOSED_SHELL('',(#6819,#6820,#6821,#6822,#6823,#6824));
#7155=CLOSED_SHELL('',(#6825,#6826,#6827,#6828,#6829,#6830,#6831,#6832,
#6833,#6834,#6835,#6836,#6837,#6838,#6839,#6840,#6841,#6842,#6843,#6844,
#6845,#6846,#6847,#6848,#6849,#6850,#6851,#6852,#6853,#6854,#6855,#6856,
#6857,#6858,#6859,#6860,#6861,#6862,#6863,#6864,#6865,#6866,#6867,#6868,
#6869,#6870,#6871,#6872,#6873,#6874,#6875,#6876,#6877,#6878,#6879,#6880,
#6881,#6882,#6883,#6884,#6885,#6886,#6887,#6888,#6889,#6890,#6891,#6892,
#6893,#6894,#6895,#6896,#6897,#6898,#6899,#6900,#6901,#6902,#6903,#6904,
#6905,#6906,#6907,#6908,#6909,#6910,#6911,#6912,#6913));
#7156=CLOSED_SHELL('',(#6914,#6915,#6916,#6917,#6918,#6919,#6920,#6921,
#6922,#6923,#6924,#6925,#6926,#6927,#6928,#6929,#6930,#6931,#6932,#6933,
#6934,#6935,#6936,#6937,#6938,#6939,#6940,#6941,#6942,#6943,#6944,#6945,
#6946,#6947,#6948,#6949,#6950,#6951,#6952,#6953,#6954,#6955,#6956,#6957,
#6958,#6959,#6960,#6961,#6962,#6963,#6964,#6965,#6966,#6967,#6968,#6969,
#6970,#6971,#6972,#6973,#6974,#6975,#6976,#6977,#6978,#6979,#6980,#6981,
#6982,#6983,#6984,#6985,#6986,#6987,#6988,#6989,#6990,#6991,#6992,#6993,
#6994,#6995,#6996,#6997,#6998,#6999,#7000,#7001,#7002,#7003,#7004,#7005,
#7006,#7007,#7008,#7009,#7010,#7011,#7012));
#7157=CLOSED_SHELL('',(#7013,#7014,#7015,#7016,#7017,#7018,#7019,#7020,
#7021,#7022,#7023,#7024,#7025,#7026,#7027,#7028,#7029,#7030,#7031,#7032,
#7033,#7034,#7035,#7036,#7037,#7038,#7039,#7040,#7041,#7042,#7043,#7044,
#7045,#7046,#7047,#7048));
#7158=CLOSED_SHELL('',(#7049,#7050,#7051,#7052,#7053,#7054,#7055,#7056,
#7057,#7058,#7059,#7060,#7061,#7062,#7063,#7064,#7065,#7066,#7067,#7068,
#7069,#7070,#7071,#7072,#7073,#7074,#7075,#7076,#7077,#7078,#7079,#7080,
#7081,#7082,#7083,#7084,#7085,#7086,#7087,#7088,#7089,#7090,#7091,#7092,
#7093,#7094,#7095,#7096,#7097,#7098,#7099,#7100,#7101,#7102,#7103,#7104,
#7105,#7106,#7107,#7108,#7109,#7110,#7111,#7112,#7113,#7114,#7115,#7116,
#7117,#7118,#7119,#7120,#7121,#7122,#7123,#7124));
#7159=CLOSED_SHELL('',(#7125,#7126,#7127,#7128,#7129,#7130,#7131,#7132,
#7133,#7134,#7135,#7136,#7137,#7138,#7139,#7140,#7141,#7142,#7143,#7144,
#7145,#7146));
#7160=CLOSED_SHELL('',(#7147,#7148,#7149,#7150));
#7161=DERIVED_UNIT_ELEMENT(#7181,1.);
#7162=DERIVED_UNIT_ELEMENT(#19473,-3.);
#7163=DERIVED_UNIT_ELEMENT(#7181,1.);
#7164=DERIVED_UNIT_ELEMENT(#19473,-3.);
#7165=DERIVED_UNIT_ELEMENT(#7181,1.);
#7166=DERIVED_UNIT_ELEMENT(#19473,-3.);
#7167=DERIVED_UNIT_ELEMENT(#7181,1.);
#7168=DERIVED_UNIT_ELEMENT(#19473,-3.);
#7169=DERIVED_UNIT_ELEMENT(#7181,1.);
#7170=DERIVED_UNIT_ELEMENT(#19473,-3.);
#7171=DERIVED_UNIT_ELEMENT(#7181,1.);
#7172=DERIVED_UNIT_ELEMENT(#19473,-3.);
#7173=DERIVED_UNIT_ELEMENT(#7181,1.);
#7174=DERIVED_UNIT_ELEMENT(#19473,-3.);
#7175=DERIVED_UNIT_ELEMENT(#7181,1.);
#7176=DERIVED_UNIT_ELEMENT(#19473,-3.);
#7177=DERIVED_UNIT_ELEMENT(#7181,1.);
#7178=DERIVED_UNIT_ELEMENT(#19473,-3.);
#7179=DERIVED_UNIT_ELEMENT(#7181,1.);
#7180=DERIVED_UNIT_ELEMENT(#19473,-3.);
#7181=(
MASS_UNIT()
NAMED_UNIT(*)
SI_UNIT(.KILO.,.GRAM.)
);
#7182=DERIVED_UNIT((#7161,#7162));
#7183=DERIVED_UNIT((#7163,#7164));
#7184=DERIVED_UNIT((#7165,#7166));
#7185=DERIVED_UNIT((#7167,#7168));
#7186=DERIVED_UNIT((#7169,#7170));
#7187=DERIVED_UNIT((#7171,#7172));
#7188=DERIVED_UNIT((#7173,#7174));
#7189=DERIVED_UNIT((#7175,#7176));
#7190=DERIVED_UNIT((#7177,#7178));
#7191=DERIVED_UNIT((#7179,#7180));
#7192=MEASURE_REPRESENTATION_ITEM('density measure',
POSITIVE_RATIO_MEASURE(7850.),#7182);
#7193=MEASURE_REPRESENTATION_ITEM('density measure',
POSITIVE_RATIO_MEASURE(7850.),#7183);
#7194=MEASURE_REPRESENTATION_ITEM('density measure',
POSITIVE_RATIO_MEASURE(7850.),#7184);
#7195=MEASURE_REPRESENTATION_ITEM('density measure',
POSITIVE_RATIO_MEASURE(7850.),#7185);
#7196=MEASURE_REPRESENTATION_ITEM('density measure',
POSITIVE_RATIO_MEASURE(7850.),#7186);
#7197=MEASURE_REPRESENTATION_ITEM('density measure',
POSITIVE_RATIO_MEASURE(7850.),#7187);
#7198=MEASURE_REPRESENTATION_ITEM('density measure',
POSITIVE_RATIO_MEASURE(7850.),#7188);
#7199=MEASURE_REPRESENTATION_ITEM('density measure',
POSITIVE_RATIO_MEASURE(7850.),#7189);
#7200=MEASURE_REPRESENTATION_ITEM('density measure',
POSITIVE_RATIO_MEASURE(7850.),#7190);
#7201=MEASURE_REPRESENTATION_ITEM('density measure',
POSITIVE_RATIO_MEASURE(7850.),#7191);
#7202=PROPERTY_DEFINITION_REPRESENTATION(#7252,#7222);
#7203=PROPERTY_DEFINITION_REPRESENTATION(#7253,#7223);
#7204=PROPERTY_DEFINITION_REPRESENTATION(#7254,#7224);
#7205=PROPERTY_DEFINITION_REPRESENTATION(#7255,#7225);
#7206=PROPERTY_DEFINITION_REPRESENTATION(#7256,#7226);
#7207=PROPERTY_DEFINITION_REPRESENTATION(#7257,#7227);
#7208=PROPERTY_DEFINITION_REPRESENTATION(#7258,#7228);
#7209=PROPERTY_DEFINITION_REPRESENTATION(#7259,#7229);
#7210=PROPERTY_DEFINITION_REPRESENTATION(#7260,#7230);
#7211=PROPERTY_DEFINITION_REPRESENTATION(#7261,#7231);
#7212=PROPERTY_DEFINITION_REPRESENTATION(#7262,#7232);
#7213=PROPERTY_DEFINITION_REPRESENTATION(#7263,#7233);
#7214=PROPERTY_DEFINITION_REPRESENTATION(#7264,#7234);
#7215=PROPERTY_DEFINITION_REPRESENTATION(#7265,#7235);
#7216=PROPERTY_DEFINITION_REPRESENTATION(#7266,#7236);
#7217=PROPERTY_DEFINITION_REPRESENTATION(#7267,#7237);
#7218=PROPERTY_DEFINITION_REPRESENTATION(#7268,#7238);
#7219=PROPERTY_DEFINITION_REPRESENTATION(#7269,#7239);
#7220=PROPERTY_DEFINITION_REPRESENTATION(#7270,#7240);
#7221=PROPERTY_DEFINITION_REPRESENTATION(#7271,#7241);
#7222=REPRESENTATION('material name',(#7242),#19460);
#7223=REPRESENTATION('density',(#7192),#19460);
#7224=REPRESENTATION('material name',(#7243),#19461);
#7225=REPRESENTATION('density',(#7193),#19461);
#7226=REPRESENTATION('material name',(#7244),#19462);
#7227=REPRESENTATION('density',(#7194),#19462);
#7228=REPRESENTATION('material name',(#7245),#19463);
#7229=REPRESENTATION('density',(#7195),#19463);
#7230=REPRESENTATION('material name',(#7246),#19465);
#7231=REPRESENTATION('density',(#7196),#19465);
#7232=REPRESENTATION('material name',(#7247),#19466);
#7233=REPRESENTATION('density',(#7197),#19466);
#7234=REPRESENTATION('material name',(#7248),#19467);
#7235=REPRESENTATION('density',(#7198),#19467);
#7236=REPRESENTATION('material name',(#7249),#19468);
#7237=REPRESENTATION('density',(#7199),#19468);
#7238=REPRESENTATION('material name',(#7250),#19469);
#7239=REPRESENTATION('density',(#7200),#19469);
#7240=REPRESENTATION('material name',(#7251),#19470);
#7241=REPRESENTATION('density',(#7201),#19470);
#7242=DESCRIPTIVE_REPRESENTATION_ITEM('Steel','Steel');
#7243=DESCRIPTIVE_REPRESENTATION_ITEM('Steel','Steel');
#7244=DESCRIPTIVE_REPRESENTATION_ITEM('Steel','Steel');
#7245=DESCRIPTIVE_REPRESENTATION_ITEM('Steel','Steel');
#7246=DESCRIPTIVE_REPRESENTATION_ITEM('Steel','Steel');
#7247=DESCRIPTIVE_REPRESENTATION_ITEM('Steel','Steel');
#7248=DESCRIPTIVE_REPRESENTATION_ITEM('Steel','Steel');
#7249=DESCRIPTIVE_REPRESENTATION_ITEM('Steel','Steel');
#7250=DESCRIPTIVE_REPRESENTATION_ITEM('Steel','Steel');
#7251=DESCRIPTIVE_REPRESENTATION_ITEM('Steel','Steel');
#7252=PROPERTY_DEFINITION('material property','material name',#19530);
#7253=PROPERTY_DEFINITION('material property','density of part',#19530);
#7254=PROPERTY_DEFINITION('material property','material name',#19531);
#7255=PROPERTY_DEFINITION('material property','density of part',#19531);
#7256=PROPERTY_DEFINITION('material property','material name',#19532);
#7257=PROPERTY_DEFINITION('material property','density of part',#19532);
#7258=PROPERTY_DEFINITION('material property','material name',#19533);
#7259=PROPERTY_DEFINITION('material property','density of part',#19533);
#7260=PROPERTY_DEFINITION('material property','material name',#19535);
#7261=PROPERTY_DEFINITION('material property','density of part',#19535);
#7262=PROPERTY_DEFINITION('material property','material name',#19536);
#7263=PROPERTY_DEFINITION('material property','density of part',#19536);
#7264=PROPERTY_DEFINITION('material property','material name',#19537);
#7265=PROPERTY_DEFINITION('material property','density of part',#19537);
#7266=PROPERTY_DEFINITION('material property','material name',#19538);
#7267=PROPERTY_DEFINITION('material property','density of part',#19538);
#7268=PROPERTY_DEFINITION('material property','material name',#19539);
#7269=PROPERTY_DEFINITION('material property','density of part',#19539);
#7270=PROPERTY_DEFINITION('material property','material name',#19540);
#7271=PROPERTY_DEFINITION('material property','density of part',#19540);
#7272=AXIS2_PLACEMENT_3D('',#9387,#7819,#7820);
#7273=AXIS2_PLACEMENT_3D('',#9388,#7821,#7822);
#7274=AXIS2_PLACEMENT_3D('',#9389,#7823,#7824);
#7275=AXIS2_PLACEMENT_3D('',#9391,#7825,#7826);
#7276=AXIS2_PLACEMENT_3D('',#9394,#7828,#7829);
#7277=AXIS2_PLACEMENT_3D('',#9395,#7830,#7831);
#7278=AXIS2_PLACEMENT_3D('',#9397,#7832,#7833);
#7279=AXIS2_PLACEMENT_3D('',#9400,#7835,#7836);
#7280=AXIS2_PLACEMENT_3D('',#9401,#7837,#7838);
#7281=AXIS2_PLACEMENT_3D('',#9403,#7839,#7840);
#7282=AXIS2_PLACEMENT_3D('',#9406,#7842,#7843);
#7283=AXIS2_PLACEMENT_3D('',#9407,#7844,#7845);
#7284=AXIS2_PLACEMENT_3D('',#9414,#7849,#7850);
#7285=AXIS2_PLACEMENT_3D('',#9420,#7854,#7855);
#7286=AXIS2_PLACEMENT_3D('',#9424,#7858,#7859);
#7287=AXIS2_PLACEMENT_3D('',#9435,#7865,#7866);
#7288=AXIS2_PLACEMENT_3D('',#9436,#7867,#7868);
#7289=AXIS2_PLACEMENT_3D('',#9440,#7871,#7872);
#7290=AXIS2_PLACEMENT_3D('',#9442,#7873,#7874);
#7291=AXIS2_PLACEMENT_3D('',#9443,#7875,#7876);
#7292=AXIS2_PLACEMENT_3D('',#9445,#7878,#7879);
#7293=AXIS2_PLACEMENT_3D('',#9447,#7880,#7881);
#7294=AXIS2_PLACEMENT_3D('',#9449,#7883,#7884);
#7295=AXIS2_PLACEMENT_3D('',#9453,#7887,#7888);
#7296=AXIS2_PLACEMENT_3D('',#9459,#7892,#7893);
#7297=AXIS2_PLACEMENT_3D('',#9467,#7898,#7899);
#7298=AXIS2_PLACEMENT_3D('',#9471,#7902,#7903);
#7299=AXIS2_PLACEMENT_3D('',#9472,#7904,#7905);
#7300=AXIS2_PLACEMENT_3D('',#9478,#7909,#7910);
#7301=AXIS2_PLACEMENT_3D('',#9482,#7912,#7913);
#7302=AXIS2_PLACEMENT_3D('',#9488,#7916,#7917);
#7303=AXIS2_PLACEMENT_3D('',#9500,#7923,#7924);
#7304=AXIS2_PLACEMENT_3D('',#9503,#7926,#7927);
#7305=AXIS2_PLACEMENT_3D('',#9505,#7928,#7929);
#7306=AXIS2_PLACEMENT_3D('',#9506,#7930,#7931);
#7307=AXIS2_PLACEMENT_3D('',#9510,#7934,#7935);
#7308=AXIS2_PLACEMENT_3D('',#9513,#7937,#7938);
#7309=AXIS2_PLACEMENT_3D('',#9514,#7939,#7940);
#7310=AXIS2_PLACEMENT_3D('',#9516,#7941,#7942);
#7311=AXIS2_PLACEMENT_3D('',#9518,#7944,#7945);
#7312=AXIS2_PLACEMENT_3D('',#9522,#7947,#7948);
#7313=AXIS2_PLACEMENT_3D('',#9534,#7954,#7955);
#7314=AXIS2_PLACEMENT_3D('',#9539,#7958,#7959);
#7315=AXIS2_PLACEMENT_3D('',#9540,#7960,#7961);
#7316=AXIS2_PLACEMENT_3D('',#9542,#7962,#7963);
#7317=AXIS2_PLACEMENT_3D('',#9543,#7964,#7965);
#7318=AXIS2_PLACEMENT_3D('',#9544,#7966,#7967);
#7319=AXIS2_PLACEMENT_3D('',#9547,#7968,#7969);
#7320=AXIS2_PLACEMENT_3D('',#9548,#7970,#7971);
#7321=AXIS2_PLACEMENT_3D('',#9550,#7973,#7974);
#7322=AXIS2_PLACEMENT_3D('',#9551,#7975,#7976);
#7323=AXIS2_PLACEMENT_3D('',#9552,#7977,#7978);
#7324=AXIS2_PLACEMENT_3D('',#9555,#7981,#7982);
#7325=AXIS2_PLACEMENT_3D('',#9558,#7985,#7986);
#7326=AXIS2_PLACEMENT_3D('',#9560,#7988,#7989);
#7327=AXIS2_PLACEMENT_3D('',#9562,#7991,#7992);
#7328=AXIS2_PLACEMENT_3D('',#9563,#7993,#7994);
#7329=AXIS2_PLACEMENT_3D('',#9565,#7996,#7997);
#7330=AXIS2_PLACEMENT_3D('',#9566,#7998,#7999);
#7331=AXIS2_PLACEMENT_3D('',#9568,#8001,#8002);
#7332=AXIS2_PLACEMENT_3D('',#9570,#8004,#8005);
#7333=AXIS2_PLACEMENT_3D('',#9571,#8006,#8007);
#7334=AXIS2_PLACEMENT_3D('',#9572,#8008,#8009);
#7335=AXIS2_PLACEMENT_3D('',#9574,#8010,#8011);
#7336=AXIS2_PLACEMENT_3D('',#9577,#8013,#8014);
#7337=AXIS2_PLACEMENT_3D('',#9578,#8015,#8016);
#7338=AXIS2_PLACEMENT_3D('',#9580,#8017,#8018);
#7339=AXIS2_PLACEMENT_3D('',#9583,#8020,#8021);
#7340=AXIS2_PLACEMENT_3D('',#9584,#8022,#8023);
#7341=AXIS2_PLACEMENT_3D('',#9586,#8024,#8025);
#7342=AXIS2_PLACEMENT_3D('',#9589,#8027,#8028);
#7343=AXIS2_PLACEMENT_3D('',#9590,#8029,#8030);
#7344=AXIS2_PLACEMENT_3D('',#9597,#8034,#8035);
#7345=AXIS2_PLACEMENT_3D('',#9603,#8039,#8040);
#7346=AXIS2_PLACEMENT_3D('',#9607,#8043,#8044);
#7347=AXIS2_PLACEMENT_3D('',#9614,#8048,#8049);
#7348=AXIS2_PLACEMENT_3D('',#9615,#8050,#8051);
#7349=AXIS2_PLACEMENT_3D('',#9616,#8052,#8053);
#7350=AXIS2_PLACEMENT_3D('',#9617,#8054,#8055);
#7351=AXIS2_PLACEMENT_3D('',#9621,#8058,#8059);
#7352=AXIS2_PLACEMENT_3D('',#9623,#8060,#8061);
#7353=AXIS2_PLACEMENT_3D('',#9625,#8063,#8064);
#7354=AXIS2_PLACEMENT_3D('',#9627,#8065,#8066);
#7355=AXIS2_PLACEMENT_3D('',#9629,#8068,#8069);
#7356=AXIS2_PLACEMENT_3D('',#9637,#8074,#8075);
#7357=AXIS2_PLACEMENT_3D('',#9643,#8079,#8080);
#7358=AXIS2_PLACEMENT_3D('',#9651,#8085,#8086);
#7359=AXIS2_PLACEMENT_3D('',#9657,#8089,#8090);
#7360=AXIS2_PLACEMENT_3D('',#9663,#8093,#8094);
#7361=AXIS2_PLACEMENT_3D('',#9675,#8100,#8101);
#7362=AXIS2_PLACEMENT_3D('',#9678,#8103,#8104);
#7363=AXIS2_PLACEMENT_3D('',#9680,#8105,#8106);
#7364=AXIS2_PLACEMENT_3D('',#9681,#8107,#8108);
#7365=AXIS2_PLACEMENT_3D('',#9687,#8112,#8113);
#7366=AXIS2_PLACEMENT_3D('',#9689,#8115,#8116);
#7367=AXIS2_PLACEMENT_3D('',#9693,#8119,#8120);
#7368=AXIS2_PLACEMENT_3D('',#9696,#8122,#8123);
#7369=AXIS2_PLACEMENT_3D('',#9697,#8124,#8125);
#7370=AXIS2_PLACEMENT_3D('',#9699,#8126,#8127);
#7371=AXIS2_PLACEMENT_3D('',#9701,#8129,#8130);
#7372=AXIS2_PLACEMENT_3D('',#9705,#8132,#8133);
#7373=AXIS2_PLACEMENT_3D('',#9717,#8139,#8140);
#7374=AXIS2_PLACEMENT_3D('',#9722,#8143,#8144);
#7375=AXIS2_PLACEMENT_3D('',#9723,#8145,#8146);
#7376=AXIS2_PLACEMENT_3D('',#9725,#8147,#8148);
#7377=AXIS2_PLACEMENT_3D('',#9726,#8149,#8150);
#7378=AXIS2_PLACEMENT_3D('',#9727,#8151,#8152);
#7379=AXIS2_PLACEMENT_3D('',#9730,#8153,#8154);
#7380=AXIS2_PLACEMENT_3D('',#9731,#8155,#8156);
#7381=AXIS2_PLACEMENT_3D('',#9733,#8158,#8159);
#7382=AXIS2_PLACEMENT_3D('',#9734,#8160,#8161);
#7383=AXIS2_PLACEMENT_3D('',#9735,#8162,#8163);
#7384=AXIS2_PLACEMENT_3D('',#9738,#8166,#8167);
#7385=AXIS2_PLACEMENT_3D('',#9741,#8170,#8171);
#7386=AXIS2_PLACEMENT_3D('',#9743,#8173,#8174);
#7387=AXIS2_PLACEMENT_3D('',#9745,#8176,#8177);
#7388=AXIS2_PLACEMENT_3D('',#9746,#8178,#8179);
#7389=AXIS2_PLACEMENT_3D('',#9748,#8181,#8182);
#7390=AXIS2_PLACEMENT_3D('',#9749,#8183,#8184);
#7391=AXIS2_PLACEMENT_3D('',#9751,#8186,#8187);
#7392=AXIS2_PLACEMENT_3D('',#9753,#8189,#8190);
#7393=AXIS2_PLACEMENT_3D('',#9754,#8191,#8192);
#7394=AXIS2_PLACEMENT_3D('',#9755,#8193,#8194);
#7395=AXIS2_PLACEMENT_3D('',#9757,#8195,#8196);
#7396=AXIS2_PLACEMENT_3D('',#9760,#8198,#8199);
#7397=AXIS2_PLACEMENT_3D('',#9761,#8200,#8201);
#7398=AXIS2_PLACEMENT_3D('',#9763,#8202,#8203);
#7399=AXIS2_PLACEMENT_3D('',#9764,#8204,#8205);
#7400=AXIS2_PLACEMENT_3D('',#9766,#8206,#8207);
#7401=AXIS2_PLACEMENT_3D('',#9767,#8208,#8209);
#7402=AXIS2_PLACEMENT_3D('',#9769,#8210,#8211);
#7403=AXIS2_PLACEMENT_3D('',#9771,#8213,#8214);
#7404=AXIS2_PLACEMENT_3D('',#9773,#8215,#8216);
#7405=AXIS2_PLACEMENT_3D('',#9775,#8217,#8218);
#7406=AXIS2_PLACEMENT_3D('',#9776,#8219,#8220);
#7407=AXIS2_PLACEMENT_3D('',#9779,#8222,#8223);
#7408=AXIS2_PLACEMENT_3D('',#9780,#8224,#8225);
#7409=AXIS2_PLACEMENT_3D('',#9781,#8226,#8227);
#7410=AXIS2_PLACEMENT_3D('',#9783,#8229,#8230);
#7411=AXIS2_PLACEMENT_3D('',#9784,#8231,#8232);
#7412=AXIS2_PLACEMENT_3D('',#9785,#8233,#8234);
#7413=AXIS2_PLACEMENT_3D('',#9794,#8239,#8240);
#7414=AXIS2_PLACEMENT_3D('',#9803,#8245,#8246);
#7415=AXIS2_PLACEMENT_3D('',#9804,#8247,#8248);
#7416=AXIS2_PLACEMENT_3D('',#9805,#8249,#8250);
#7417=AXIS2_PLACEMENT_3D('',#9806,#8251,#8252);
#7418=AXIS2_PLACEMENT_3D('',#9807,#8253,#8254);
#7419=AXIS2_PLACEMENT_3D('',#9808,#8255,#8256);
#7420=AXIS2_PLACEMENT_3D('',#9809,#8257,#8258);
#7421=AXIS2_PLACEMENT_3D('',#9810,#8259,#8260);
#7422=AXIS2_PLACEMENT_3D('',#9811,#8261,#8262);
#7423=AXIS2_PLACEMENT_3D('',#9812,#8263,#8264);
#7424=AXIS2_PLACEMENT_3D('',#9813,#8265,#8266);
#7425=AXIS2_PLACEMENT_3D('',#9815,#8267,#8268);
#7426=AXIS2_PLACEMENT_3D('',#9818,#8270,#8271);
#7427=AXIS2_PLACEMENT_3D('',#9819,#8272,#8273);
#7428=AXIS2_PLACEMENT_3D('',#9821,#8274,#8275);
#7429=AXIS2_PLACEMENT_3D('',#9824,#8277,#8278);
#7430=AXIS2_PLACEMENT_3D('',#9825,#8279,#8280);
#7431=AXIS2_PLACEMENT_3D('',#9827,#8281,#8282);
#7432=AXIS2_PLACEMENT_3D('',#9830,#8284,#8285);
#7433=AXIS2_PLACEMENT_3D('',#9831,#8286,#8287);
#7434=AXIS2_PLACEMENT_3D('',#9833,#8288,#8289);
#7435=AXIS2_PLACEMENT_3D('',#9836,#8291,#8292);
#7436=AXIS2_PLACEMENT_3D('',#9837,#8293,#8294);
#7437=AXIS2_PLACEMENT_3D('',#9839,#8295,#8296);
#7438=AXIS2_PLACEMENT_3D('',#9842,#8298,#8299);
#7439=AXIS2_PLACEMENT_3D('',#9843,#8300,#8301);
#7440=AXIS2_PLACEMENT_3D('',#9845,#8302,#8303);
#7441=AXIS2_PLACEMENT_3D('',#9846,#8304,#8305);
#7442=AXIS2_PLACEMENT_3D('',#9848,#8306,#8307);
#7443=AXIS2_PLACEMENT_3D('',#9851,#8309,#8310);
#7444=AXIS2_PLACEMENT_3D('',#9852,#8311,#8312);
#7445=AXIS2_PLACEMENT_3D('',#9854,#8313,#8314);
#7446=AXIS2_PLACEMENT_3D('',#9855,#8315,#8316);
#7447=AXIS2_PLACEMENT_3D('',#9858,#8318,#8319);
#7448=AXIS2_PLACEMENT_3D('',#9859,#8320,#8321);
#7449=AXIS2_PLACEMENT_3D('',#9862,#8323,#8324);
#7450=AXIS2_PLACEMENT_3D('',#9863,#8325,#8326);
#7451=AXIS2_PLACEMENT_3D('',#9872,#8331,#8332);
#7452=AXIS2_PLACEMENT_3D('',#9881,#8337,#8338);
#7453=AXIS2_PLACEMENT_3D('',#9890,#8343,#8344);
#7454=AXIS2_PLACEMENT_3D('',#9899,#8349,#8350);
#7455=AXIS2_PLACEMENT_3D('',#9908,#8355,#8356);
#7456=AXIS2_PLACEMENT_3D('',#9917,#8361,#8362);
#7457=AXIS2_PLACEMENT_3D('',#9926,#8367,#8368);
#7458=AXIS2_PLACEMENT_3D('',#9928,#8369,#8370);
#7459=AXIS2_PLACEMENT_3D('',#9929,#8371,#8372);
#7460=AXIS2_PLACEMENT_3D('',#9931,#8373,#8374);
#7461=AXIS2_PLACEMENT_3D('',#9932,#8375,#8376);
#7462=AXIS2_PLACEMENT_3D('',#9935,#8379,#8380);
#7463=AXIS2_PLACEMENT_3D('',#9938,#8383,#8384);
#7464=AXIS2_PLACEMENT_3D('',#9941,#8387,#8388);
#7465=AXIS2_PLACEMENT_3D('',#9947,#8392,#8393);
#7466=AXIS2_PLACEMENT_3D('',#9953,#8397,#8398);
#7467=AXIS2_PLACEMENT_3D('',#10030,#8401,#8402);
#7468=AXIS2_PLACEMENT_3D('',#10108,#8406,#8407);
#7469=AXIS2_PLACEMENT_3D('',#10186,#8411,#8412);
#7470=AXIS2_PLACEMENT_3D('',#10264,#8416,#8417);
#7471=AXIS2_PLACEMENT_3D('',#10280,#8421,#8422);
#7472=AXIS2_PLACEMENT_3D('',#10604,#8434,#8435);
#7473=AXIS2_PLACEMENT_3D('',#10606,#8436,#8437);
#7474=AXIS2_PLACEMENT_3D('',#10608,#8439,#8440);
#7475=AXIS2_PLACEMENT_3D('',#10610,#8441,#8442);
#7476=AXIS2_PLACEMENT_3D('',#10612,#8444,#8445);
#7477=AXIS2_PLACEMENT_3D('',#10780,#8447,#8448);
#7478=AXIS2_PLACEMENT_3D('',#10781,#8449,#8450);
#7479=AXIS2_PLACEMENT_3D('',#10786,#8451,#8452);
#7480=AXIS2_PLACEMENT_3D('',#10858,#8454,#8455);
#7481=AXIS2_PLACEMENT_3D('',#10976,#8457,#8458);
#7482=AXIS2_PLACEMENT_3D('',#11021,#8459,#8460);
#7483=AXIS2_PLACEMENT_3D('',#11139,#8462,#8463);
#7484=AXIS2_PLACEMENT_3D('',#11184,#8464,#8465);
#7485=AXIS2_PLACEMENT_3D('',#11304,#8467,#8468);
#7486=AXIS2_PLACEMENT_3D('',#11309,#8469,#8470);
#7487=AXIS2_PLACEMENT_3D('',#11361,#8472,#8473);
#7488=AXIS2_PLACEMENT_3D('',#11362,#8474,#8475);
#7489=AXIS2_PLACEMENT_3D('',#11363,#8476,#8477);
#7490=AXIS2_PLACEMENT_3D('',#11364,#8478,#8479);
#7491=AXIS2_PLACEMENT_3D('',#11365,#8480,#8481);
#7492=AXIS2_PLACEMENT_3D('',#11366,#8482,#8483);
#7493=AXIS2_PLACEMENT_3D('',#11368,#8484,#8485);
#7494=AXIS2_PLACEMENT_3D('',#11369,#8486,#8487);
#7495=AXIS2_PLACEMENT_3D('',#11370,#8488,#8489);
#7496=AXIS2_PLACEMENT_3D('',#11371,#8490,#8491);
#7497=AXIS2_PLACEMENT_3D('',#11372,#8492,#8493);
#7498=AXIS2_PLACEMENT_3D('',#11373,#8494,#8495);
#7499=AXIS2_PLACEMENT_3D('',#11394,#8496,#8497);
#7500=AXIS2_PLACEMENT_3D('',#11396,#8498,#8499);
#7501=AXIS2_PLACEMENT_3D('',#11397,#8500,#8501);
#7502=AXIS2_PLACEMENT_3D('',#11398,#8502,#8503);
#7503=AXIS2_PLACEMENT_3D('',#11488,#8505,#8506);
#7504=AXIS2_PLACEMENT_3D('',#11489,#8507,#8508);
#7505=AXIS2_PLACEMENT_3D('',#11492,#8509,#8510);
#7506=AXIS2_PLACEMENT_3D('',#11494,#8511,#8512);
#7507=AXIS2_PLACEMENT_3D('',#11495,#8513,#8514);
#7508=AXIS2_PLACEMENT_3D('',#11496,#8515,#8516);
#7509=AXIS2_PLACEMENT_3D('',#11499,#8517,#8518);
#7510=AXIS2_PLACEMENT_3D('',#11501,#8519,#8520);
#7511=AXIS2_PLACEMENT_3D('',#11502,#8521,#8522);
#7512=AXIS2_PLACEMENT_3D('',#11503,#8523,#8524);
#7513=AXIS2_PLACEMENT_3D('',#11506,#8525,#8526);
#7514=AXIS2_PLACEMENT_3D('',#11508,#8527,#8528);
#7515=AXIS2_PLACEMENT_3D('',#11509,#8529,#8530);
#7516=AXIS2_PLACEMENT_3D('',#11510,#8531,#8532);
#7517=AXIS2_PLACEMENT_3D('',#11541,#8535,#8536);
#7518=AXIS2_PLACEMENT_3D('',#11544,#8537,#8538);
#7519=AXIS2_PLACEMENT_3D('',#11546,#8539,#8540);
#7520=AXIS2_PLACEMENT_3D('',#11547,#8541,#8542);
#7521=AXIS2_PLACEMENT_3D('',#11548,#8543,#8544);
#7522=AXIS2_PLACEMENT_3D('',#11728,#8547,#8548);
#7523=AXIS2_PLACEMENT_3D('',#11729,#8549,#8550);
#7524=AXIS2_PLACEMENT_3D('',#11746,#8551,#8552);
#7525=AXIS2_PLACEMENT_3D('',#11747,#8553,#8554);
#7526=AXIS2_PLACEMENT_3D('',#11748,#8555,#8556);
#7527=AXIS2_PLACEMENT_3D('',#11750,#8557,#8558);
#7528=AXIS2_PLACEMENT_3D('',#11753,#8560,#8561);
#7529=AXIS2_PLACEMENT_3D('',#11754,#8562,#8563);
#7530=AXIS2_PLACEMENT_3D('',#11756,#8564,#8565);
#7531=AXIS2_PLACEMENT_3D('',#11759,#8567,#8568);
#7532=AXIS2_PLACEMENT_3D('',#11760,#8569,#8570);
#7533=AXIS2_PLACEMENT_3D('',#11762,#8571,#8572);
#7534=AXIS2_PLACEMENT_3D('',#11765,#8574,#8575);
#7535=AXIS2_PLACEMENT_3D('',#11766,#8576,#8577);
#7536=AXIS2_PLACEMENT_3D('',#11768,#8578,#8579);
#7537=AXIS2_PLACEMENT_3D('',#11771,#8581,#8582);
#7538=AXIS2_PLACEMENT_3D('',#11772,#8583,#8584);
#7539=AXIS2_PLACEMENT_3D('',#11781,#8589,#8590);
#7540=AXIS2_PLACEMENT_3D('',#11787,#8594,#8595);
#7541=AXIS2_PLACEMENT_3D('',#11793,#8599,#8600);
#7542=AXIS2_PLACEMENT_3D('',#11799,#8604,#8605);
#7543=AXIS2_PLACEMENT_3D('',#11805,#8609,#8610);
#7544=AXIS2_PLACEMENT_3D('',#11808,#8613,#8614);
#7545=AXIS2_PLACEMENT_3D('',#11810,#8615,#8616);
#7546=AXIS2_PLACEMENT_3D('',#11811,#8617,#8618);
#7547=AXIS2_PLACEMENT_3D('',#11820,#8623,#8624);
#7548=AXIS2_PLACEMENT_3D('',#11826,#8628,#8629);
#7549=AXIS2_PLACEMENT_3D('',#11832,#8633,#8634);
#7550=AXIS2_PLACEMENT_3D('',#11838,#8638,#8639);
#7551=AXIS2_PLACEMENT_3D('',#11844,#8643,#8644);
#7552=AXIS2_PLACEMENT_3D('',#11847,#8647,#8648);
#7553=AXIS2_PLACEMENT_3D('',#11849,#8649,#8650);
#7554=AXIS2_PLACEMENT_3D('',#11850,#8651,#8652);
#7555=AXIS2_PLACEMENT_3D('',#11853,#8654,#8655);
#7556=AXIS2_PLACEMENT_3D('',#11854,#8656,#8657);
#7557=AXIS2_PLACEMENT_3D('',#11857,#8659,#8660);
#7558=AXIS2_PLACEMENT_3D('',#11858,#8661,#8662);
#7559=AXIS2_PLACEMENT_3D('',#11867,#8667,#8668);
#7560=AXIS2_PLACEMENT_3D('',#11876,#8673,#8674);
#7561=AXIS2_PLACEMENT_3D('',#11885,#8679,#8680);
#7562=AXIS2_PLACEMENT_3D('',#11894,#8685,#8686);
#7563=AXIS2_PLACEMENT_3D('',#11903,#8691,#8692);
#7564=AXIS2_PLACEMENT_3D('',#11912,#8697,#8698);
#7565=AXIS2_PLACEMENT_3D('',#11921,#8703,#8704);
#7566=AXIS2_PLACEMENT_3D('',#11923,#8705,#8706);
#7567=AXIS2_PLACEMENT_3D('',#11924,#8707,#8708);
#7568=AXIS2_PLACEMENT_3D('',#11926,#8709,#8710);
#7569=AXIS2_PLACEMENT_3D('',#11927,#8711,#8712);
#7570=AXIS2_PLACEMENT_3D('',#11930,#8715,#8716);
#7571=AXIS2_PLACEMENT_3D('',#11933,#8719,#8720);
#7572=AXIS2_PLACEMENT_3D('',#11936,#8723,#8724);
#7573=AXIS2_PLACEMENT_3D('',#11942,#8728,#8729);
#7574=AXIS2_PLACEMENT_3D('',#11948,#8733,#8734);
#7575=AXIS2_PLACEMENT_3D('',#12025,#8737,#8738);
#7576=AXIS2_PLACEMENT_3D('',#12103,#8742,#8743);
#7577=AXIS2_PLACEMENT_3D('',#12181,#8747,#8748);
#7578=AXIS2_PLACEMENT_3D('',#12259,#8752,#8753);
#7579=AXIS2_PLACEMENT_3D('',#12275,#8757,#8758);
#7580=AXIS2_PLACEMENT_3D('',#12599,#8770,#8771);
#7581=AXIS2_PLACEMENT_3D('',#12601,#8772,#8773);
#7582=AXIS2_PLACEMENT_3D('',#12603,#8775,#8776);
#7583=AXIS2_PLACEMENT_3D('',#12605,#8777,#8778);
#7584=AXIS2_PLACEMENT_3D('',#12607,#8780,#8781);
#7585=AXIS2_PLACEMENT_3D('',#12775,#8783,#8784);
#7586=AXIS2_PLACEMENT_3D('',#12776,#8785,#8786);
#7587=AXIS2_PLACEMENT_3D('',#12781,#8787,#8788);
#7588=AXIS2_PLACEMENT_3D('',#12853,#8790,#8791);
#7589=AXIS2_PLACEMENT_3D('',#12971,#8793,#8794);
#7590=AXIS2_PLACEMENT_3D('',#13016,#8795,#8796);
#7591=AXIS2_PLACEMENT_3D('',#13134,#8798,#8799);
#7592=AXIS2_PLACEMENT_3D('',#13179,#8800,#8801);
#7593=AXIS2_PLACEMENT_3D('',#13299,#8803,#8804);
#7594=AXIS2_PLACEMENT_3D('',#13304,#8805,#8806);
#7595=AXIS2_PLACEMENT_3D('',#13356,#8808,#8809);
#7596=AXIS2_PLACEMENT_3D('',#13357,#8810,#8811);
#7597=AXIS2_PLACEMENT_3D('',#13358,#8812,#8813);
#7598=AXIS2_PLACEMENT_3D('',#13359,#8814,#8815);
#7599=AXIS2_PLACEMENT_3D('',#13360,#8816,#8817);
#7600=AXIS2_PLACEMENT_3D('',#13361,#8818,#8819);
#7601=AXIS2_PLACEMENT_3D('',#13363,#8820,#8821);
#7602=AXIS2_PLACEMENT_3D('',#13364,#8822,#8823);
#7603=AXIS2_PLACEMENT_3D('',#13365,#8824,#8825);
#7604=AXIS2_PLACEMENT_3D('',#13366,#8826,#8827);
#7605=AXIS2_PLACEMENT_3D('',#13367,#8828,#8829);
#7606=AXIS2_PLACEMENT_3D('',#13368,#8830,#8831);
#7607=AXIS2_PLACEMENT_3D('',#13389,#8832,#8833);
#7608=AXIS2_PLACEMENT_3D('',#13391,#8834,#8835);
#7609=AXIS2_PLACEMENT_3D('',#13392,#8836,#8837);
#7610=AXIS2_PLACEMENT_3D('',#13393,#8838,#8839);
#7611=AXIS2_PLACEMENT_3D('',#13483,#8841,#8842);
#7612=AXIS2_PLACEMENT_3D('',#13484,#8843,#8844);
#7613=AXIS2_PLACEMENT_3D('',#13487,#8845,#8846);
#7614=AXIS2_PLACEMENT_3D('',#13489,#8847,#8848);
#7615=AXIS2_PLACEMENT_3D('',#13490,#8849,#8850);
#7616=AXIS2_PLACEMENT_3D('',#13491,#8851,#8852);
#7617=AXIS2_PLACEMENT_3D('',#13494,#8853,#8854);
#7618=AXIS2_PLACEMENT_3D('',#13496,#8855,#8856);
#7619=AXIS2_PLACEMENT_3D('',#13497,#8857,#8858);
#7620=AXIS2_PLACEMENT_3D('',#13498,#8859,#8860);
#7621=AXIS2_PLACEMENT_3D('',#13501,#8861,#8862);
#7622=AXIS2_PLACEMENT_3D('',#13503,#8863,#8864);
#7623=AXIS2_PLACEMENT_3D('',#13504,#8865,#8866);
#7624=AXIS2_PLACEMENT_3D('',#13505,#8867,#8868);
#7625=AXIS2_PLACEMENT_3D('',#13536,#8871,#8872);
#7626=AXIS2_PLACEMENT_3D('',#13539,#8873,#8874);
#7627=AXIS2_PLACEMENT_3D('',#13541,#8875,#8876);
#7628=AXIS2_PLACEMENT_3D('',#13542,#8877,#8878);
#7629=AXIS2_PLACEMENT_3D('',#13543,#8879,#8880);
#7630=AXIS2_PLACEMENT_3D('',#13723,#8883,#8884);
#7631=AXIS2_PLACEMENT_3D('',#13724,#8885,#8886);
#7632=AXIS2_PLACEMENT_3D('',#13741,#8887,#8888);
#7633=AXIS2_PLACEMENT_3D('',#13742,#8889,#8890);
#7634=AXIS2_PLACEMENT_3D('',#13743,#8891,#8892);
#7635=AXIS2_PLACEMENT_3D('',#13745,#8893,#8894);
#7636=AXIS2_PLACEMENT_3D('',#13748,#8896,#8897);
#7637=AXIS2_PLACEMENT_3D('',#13749,#8898,#8899);
#7638=AXIS2_PLACEMENT_3D('',#13751,#8900,#8901);
#7639=AXIS2_PLACEMENT_3D('',#13754,#8903,#8904);
#7640=AXIS2_PLACEMENT_3D('',#13755,#8905,#8906);
#7641=AXIS2_PLACEMENT_3D('',#13757,#8907,#8908);
#7642=AXIS2_PLACEMENT_3D('',#13759,#8909,#8910);
#7643=AXIS2_PLACEMENT_3D('',#13760,#8911,#8912);
#7644=AXIS2_PLACEMENT_3D('',#13762,#8913,#8914);
#7645=AXIS2_PLACEMENT_3D('',#13764,#8916,#8917);
#7646=AXIS2_PLACEMENT_3D('',#13765,#8918,#8919);
#7647=AXIS2_PLACEMENT_3D('',#13767,#8920,#8921);
#7648=AXIS2_PLACEMENT_3D('',#13769,#8922,#8923);
#7649=AXIS2_PLACEMENT_3D('',#13770,#8924,#8925);
#7650=AXIS2_PLACEMENT_3D('',#13772,#8926,#8927);
#7651=AXIS2_PLACEMENT_3D('',#13774,#8929,#8930);
#7652=AXIS2_PLACEMENT_3D('',#13775,#8931,#8932);
#7653=AXIS2_PLACEMENT_3D('',#13777,#8933,#8934);
#7654=AXIS2_PLACEMENT_3D('',#13779,#8935,#8936);
#7655=AXIS2_PLACEMENT_3D('',#13780,#8937,#8938);
#7656=AXIS2_PLACEMENT_3D('',#13782,#8939,#8940);
#7657=AXIS2_PLACEMENT_3D('',#13784,#8942,#8943);
#7658=AXIS2_PLACEMENT_3D('',#13785,#8944,#8945);
#7659=AXIS2_PLACEMENT_3D('',#13787,#8946,#8947);
#7660=AXIS2_PLACEMENT_3D('',#13789,#8948,#8949);
#7661=AXIS2_PLACEMENT_3D('',#13790,#8950,#8951);
#7662=AXIS2_PLACEMENT_3D('',#13792,#8952,#8953);
#7663=AXIS2_PLACEMENT_3D('',#13794,#8955,#8956);
#7664=AXIS2_PLACEMENT_3D('',#13795,#8957,#8958);
#7665=AXIS2_PLACEMENT_3D('',#13798,#8960,#8961);
#7666=AXIS2_PLACEMENT_3D('',#13799,#8962,#8963);
#7667=AXIS2_PLACEMENT_3D('',#13802,#8965,#8966);
#7668=AXIS2_PLACEMENT_3D('',#13803,#8967,#8968);
#7669=AXIS2_PLACEMENT_3D('',#13806,#8970,#8971);
#7670=AXIS2_PLACEMENT_3D('',#13807,#8972,#8973);
#7671=AXIS2_PLACEMENT_3D('',#13810,#8975,#8976);
#7672=AXIS2_PLACEMENT_3D('',#13838,#8977,#8978);
#7673=AXIS2_PLACEMENT_3D('',#13846,#8979,#8980);
#7674=AXIS2_PLACEMENT_3D('',#13852,#8981,#8982);
#7675=AXIS2_PLACEMENT_3D('',#13855,#8983,#8984);
#7676=AXIS2_PLACEMENT_3D('',#13885,#8987,#8988);
#7677=AXIS2_PLACEMENT_3D('',#13928,#8989,#8990);
#7678=AXIS2_PLACEMENT_3D('',#13968,#8991,#8992);
#7679=AXIS2_PLACEMENT_3D('',#13979,#8993,#8994);
#7680=AXIS2_PLACEMENT_3D('',#13982,#8995,#8996);
#7681=AXIS2_PLACEMENT_3D('',#14012,#8999,#9000);
#7682=AXIS2_PLACEMENT_3D('',#14065,#9001,#9002);
#7683=AXIS2_PLACEMENT_3D('',#14205,#9004,#9005);
#7684=AXIS2_PLACEMENT_3D('',#14206,#9006,#9007);
#7685=AXIS2_PLACEMENT_3D('',#14316,#9009,#9010);
#7686=AXIS2_PLACEMENT_3D('',#14337,#9011,#9012);
#7687=AXIS2_PLACEMENT_3D('',#14338,#9013,#9014);
#7688=AXIS2_PLACEMENT_3D('',#14354,#9016,#9017);
#7689=AXIS2_PLACEMENT_3D('',#14362,#9018,#9019);
#7690=AXIS2_PLACEMENT_3D('',#14410,#9021,#9022);
#7691=AXIS2_PLACEMENT_3D('',#14458,#9024,#9025);
#7692=AXIS2_PLACEMENT_3D('',#14509,#9027,#9028);
#7693=AXIS2_PLACEMENT_3D('',#14557,#9030,#9031);
#7694=AXIS2_PLACEMENT_3D('',#14605,#9033,#9034);
#7695=AXIS2_PLACEMENT_3D('',#14653,#9036,#9037);
#7696=AXIS2_PLACEMENT_3D('',#14707,#9039,#9040);
#7697=AXIS2_PLACEMENT_3D('',#14755,#9042,#9043);
#7698=AXIS2_PLACEMENT_3D('',#14803,#9045,#9046);
#7699=AXIS2_PLACEMENT_3D('',#14857,#9048,#9049);
#7700=AXIS2_PLACEMENT_3D('',#14905,#9051,#9052);
#7701=AXIS2_PLACEMENT_3D('',#14953,#9054,#9055);
#7702=AXIS2_PLACEMENT_3D('',#15001,#9057,#9058);
#7703=AXIS2_PLACEMENT_3D('',#15055,#9060,#9061);
#7704=AXIS2_PLACEMENT_3D('',#15103,#9063,#9064);
#7705=AXIS2_PLACEMENT_3D('',#15151,#9066,#9067);
#7706=AXIS2_PLACEMENT_3D('',#15205,#9069,#9070);
#7707=AXIS2_PLACEMENT_3D('',#15253,#9072,#9073);
#7708=AXIS2_PLACEMENT_3D('',#15301,#9075,#9076);
#7709=AXIS2_PLACEMENT_3D('',#15355,#9078,#9079);
#7710=AXIS2_PLACEMENT_3D('',#15403,#9081,#9082);
#7711=AXIS2_PLACEMENT_3D('',#15451,#9084,#9085);
#7712=AXIS2_PLACEMENT_3D('',#15499,#9087,#9088);
#7713=AXIS2_PLACEMENT_3D('',#15553,#9090,#9091);
#7714=AXIS2_PLACEMENT_3D('',#15601,#9093,#9094);
#7715=AXIS2_PLACEMENT_3D('',#15649,#9096,#9097);
#7716=AXIS2_PLACEMENT_3D('',#15703,#9099,#9100);
#7717=AXIS2_PLACEMENT_3D('',#15751,#9102,#9103);
#7718=AXIS2_PLACEMENT_3D('',#15799,#9105,#9106);
#7719=AXIS2_PLACEMENT_3D('',#15815,#9108,#9109);
#7720=AXIS2_PLACEMENT_3D('',#15825,#9110,#9111);
#7721=AXIS2_PLACEMENT_3D('',#15849,#9113,#9114);
#7722=AXIS2_PLACEMENT_3D('',#15873,#9116,#9117);
#7723=AXIS2_PLACEMENT_3D('',#15898,#9119,#9120);
#7724=AXIS2_PLACEMENT_3D('',#15923,#9122,#9123);
#7725=AXIS2_PLACEMENT_3D('',#15947,#9125,#9126);
#7726=AXIS2_PLACEMENT_3D('',#15972,#9128,#9129);
#7727=AXIS2_PLACEMENT_3D('',#15997,#9131,#9132);
#7728=AXIS2_PLACEMENT_3D('',#16021,#9134,#9135);
#7729=AXIS2_PLACEMENT_3D('',#16045,#9137,#9138);
#7730=AXIS2_PLACEMENT_3D('',#16070,#9140,#9141);
#7731=AXIS2_PLACEMENT_3D('',#16095,#9143,#9144);
#7732=AXIS2_PLACEMENT_3D('',#16119,#9146,#9147);
#7733=AXIS2_PLACEMENT_3D('',#16144,#9149,#9150);
#7734=AXIS2_PLACEMENT_3D('',#16169,#9152,#9153);
#7735=AXIS2_PLACEMENT_3D('',#16193,#9155,#9156);
#7736=AXIS2_PLACEMENT_3D('',#16218,#9158,#9159);
#7737=AXIS2_PLACEMENT_3D('',#16243,#9161,#9162);
#7738=AXIS2_PLACEMENT_3D('',#16267,#9164,#9165);
#7739=AXIS2_PLACEMENT_3D('',#16291,#9167,#9168);
#7740=AXIS2_PLACEMENT_3D('',#16316,#9170,#9171);
#7741=AXIS2_PLACEMENT_3D('',#16341,#9173,#9174);
#7742=AXIS2_PLACEMENT_3D('',#16365,#9176,#9177);
#7743=AXIS2_PLACEMENT_3D('',#16390,#9179,#9180);
#7744=AXIS2_PLACEMENT_3D('',#16415,#9182,#9183);
#7745=AXIS2_PLACEMENT_3D('',#16439,#9185,#9186);
#7746=AXIS2_PLACEMENT_3D('',#16464,#9188,#9189);
#7747=AXIS2_PLACEMENT_3D('',#16488,#9191,#9192);
#7748=AXIS2_PLACEMENT_3D('',#16513,#9194,#9195);
#7749=AXIS2_PLACEMENT_3D('',#16537,#9197,#9198);
#7750=AXIS2_PLACEMENT_3D('',#16699,#9199,#9200);
#7751=AXIS2_PLACEMENT_3D('',#16718,#9202,#9203);
#7752=AXIS2_PLACEMENT_3D('',#17580,#9204,#9205);
#7753=AXIS2_PLACEMENT_3D('',#17591,#9206,#9207);
#7754=AXIS2_PLACEMENT_3D('',#18458,#9208,#9209);
#7755=AXIS2_PLACEMENT_3D('',#18459,#9210,#9211);
#7756=AXIS2_PLACEMENT_3D('',#18468,#9216,#9217);
#7757=AXIS2_PLACEMENT_3D('',#18474,#9221,#9222);
#7758=AXIS2_PLACEMENT_3D('',#18480,#9226,#9227);
#7759=AXIS2_PLACEMENT_3D('',#18486,#9231,#9232);
#7760=AXIS2_PLACEMENT_3D('',#18492,#9236,#9237);
#7761=AXIS2_PLACEMENT_3D('',#18495,#9240,#9241);
#7762=AXIS2_PLACEMENT_3D('',#18496,#9242,#9243);
#7763=AXIS2_PLACEMENT_3D('',#18498,#9244,#9245);
#7764=AXIS2_PLACEMENT_3D('',#18499,#9246,#9247);
#7765=AXIS2_PLACEMENT_3D('',#18502,#9249,#9250);
#7766=AXIS2_PLACEMENT_3D('',#18503,#9251,#9252);
#7767=AXIS2_PLACEMENT_3D('',#18504,#9253,#9254);
#7768=AXIS2_PLACEMENT_3D('',#18505,#9255,#9256);
#7769=AXIS2_PLACEMENT_3D('',#18506,#9257,#9258);
#7770=AXIS2_PLACEMENT_3D('',#18511,#9260,#9261);
#7771=AXIS2_PLACEMENT_3D('',#18519,#9262,#9263);
#7772=AXIS2_PLACEMENT_3D('',#18543,#9265,#9266);
#7773=AXIS2_PLACEMENT_3D('',#18566,#9267,#9268);
#7774=AXIS2_PLACEMENT_3D('',#18620,#9270,#9271);
#7775=AXIS2_PLACEMENT_3D('',#18668,#9273,#9274);
#7776=AXIS2_PLACEMENT_3D('',#18687,#9276,#9277);
#7777=AXIS2_PLACEMENT_3D('',#18707,#9278,#9279);
#7778=AXIS2_PLACEMENT_3D('',#18720,#9281,#9282);
#7779=AXIS2_PLACEMENT_3D('',#18728,#9283,#9284);
#7780=AXIS2_PLACEMENT_3D('',#18753,#9286,#9287);
#7781=AXIS2_PLACEMENT_3D('',#18778,#9289,#9290);
#7782=AXIS2_PLACEMENT_3D('',#18803,#9292,#9293);
#7783=AXIS2_PLACEMENT_3D('',#18814,#9295,#9296);
#7784=AXIS2_PLACEMENT_3D('',#18820,#9297,#9298);
#7785=AXIS2_PLACEMENT_3D('',#19376,#9299,#9300);
#7786=AXIS2_PLACEMENT_3D('',#19389,#9307,#9308);
#7787=AXIS2_PLACEMENT_3D('',#19390,#9309,#9310);
#7788=AXIS2_PLACEMENT_3D('',#19396,#9314,#9315);
#7789=AXIS2_PLACEMENT_3D('',#19400,#9318,#9319);
#7790=AXIS2_PLACEMENT_3D('',#19404,#9322,#9323);
#7791=AXIS2_PLACEMENT_3D('',#19408,#9326,#9327);
#7792=AXIS2_PLACEMENT_3D('',#19412,#9330,#9331);
#7793=AXIS2_PLACEMENT_3D('',#19414,#9333,#9334);
#7794=AXIS2_PLACEMENT_3D('',#19415,#9335,#9336);
#7795=AXIS2_PLACEMENT_3D('',#19416,#9337,#9338);
#7796=AXIS2_PLACEMENT_3D('',#19417,#9339,#9340);
#7797=AXIS2_PLACEMENT_3D('',#19418,#9341,#9342);
#7798=AXIS2_PLACEMENT_3D('',#19419,#9343,#9344);
#7799=AXIS2_PLACEMENT_3D('',#19420,#9345,#9346);
#7800=AXIS2_PLACEMENT_3D('',#19421,#9347,#9348);
#7801=AXIS2_PLACEMENT_3D('',#19422,#9349,#9350);
#7802=AXIS2_PLACEMENT_3D('',#19423,#9351,#9352);
#7803=AXIS2_PLACEMENT_3D('',#19424,#9353,#9354);
#7804=AXIS2_PLACEMENT_3D('',#19426,#9355,#9356);
#7805=AXIS2_PLACEMENT_3D('',#19429,#9358,#9359);
#7806=AXIS2_PLACEMENT_3D('',#19430,#9360,#9361);
#7807=AXIS2_PLACEMENT_3D('',#19432,#9362,#9363);
#7808=AXIS2_PLACEMENT_3D('',#19435,#9365,#9366);
#7809=AXIS2_PLACEMENT_3D('',#19436,#9367,#9368);
#7810=AXIS2_PLACEMENT_3D('',#19437,#9369,#9370);
#7811=AXIS2_PLACEMENT_3D('',#19438,#9371,#9372);
#7812=AXIS2_PLACEMENT_3D('',#19439,#9373,#9374);
#7813=AXIS2_PLACEMENT_3D('',#19440,#9375,#9376);
#7814=AXIS2_PLACEMENT_3D('',#19441,#9377,#9378);
#7815=AXIS2_PLACEMENT_3D('',#19442,#9379,#9380);
#7816=AXIS2_PLACEMENT_3D('',#19443,#9381,#9382);
#7817=AXIS2_PLACEMENT_3D('',#19444,#9383,#9384);
#7818=AXIS2_PLACEMENT_3D('',#19445,#9385,#9386);
#7819=DIRECTION('axis',(0.,0.,1.));
#7820=DIRECTION('refdir',(1.,0.,0.));
#7821=DIRECTION('axis',(0.,0.,1.));
#7822=DIRECTION('refdir',(1.,0.,0.));
#7823=DIRECTION('center_axis',(0.,0.,-1.));
#7824=DIRECTION('ref_axis',(1.,0.,0.));
#7825=DIRECTION('center_axis',(0.,0.,-1.));
#7826=DIRECTION('ref_axis',(1.,0.,0.));
#7827=DIRECTION('',(0.,0.,-1.));
#7828=DIRECTION('center_axis',(0.,0.,1.));
#7829=DIRECTION('ref_axis',(1.,0.,0.));
#7830=DIRECTION('center_axis',(0.,0.,-1.));
#7831=DIRECTION('ref_axis',(1.,0.,0.));
#7832=DIRECTION('center_axis',(0.,0.,-1.));
#7833=DIRECTION('ref_axis',(1.,0.,0.));
#7834=DIRECTION('',(0.,0.,-1.));
#7835=DIRECTION('center_axis',(0.,0.,1.));
#7836=DIRECTION('ref_axis',(1.,0.,0.));
#7837=DIRECTION('center_axis',(0.,0.,-1.));
#7838=DIRECTION('ref_axis',(1.,0.,0.));
#7839=DIRECTION('center_axis',(0.,0.,-1.));
#7840=DIRECTION('ref_axis',(1.,0.,0.));
#7841=DIRECTION('',(0.,0.,-1.));
#7842=DIRECTION('center_axis',(0.,0.,1.));
#7843=DIRECTION('ref_axis',(1.,0.,0.));
#7844=DIRECTION('center_axis',(1.,0.,0.));
#7845=DIRECTION('ref_axis',(0.,0.,-1.));
#7846=DIRECTION('',(0.,-1.,0.));
#7847=DIRECTION('',(0.,0.8,0.6));
#7848=DIRECTION('',(0.,0.,1.));
#7849=DIRECTION('center_axis',(0.,0.6,-0.8));
#7850=DIRECTION('ref_axis',(0.,0.8,0.6));
#7851=DIRECTION('',(0.,0.8,0.6));
#7852=DIRECTION('',(-1.,0.,0.));
#7853=DIRECTION('',(1.,0.,0.));
#7854=DIRECTION('center_axis',(1.,0.,0.));
#7855=DIRECTION('ref_axis',(0.,2.22044604925031E-16,1.));
#7856=DIRECTION('',(0.,1.,0.));
#7857=DIRECTION('',(0.,0.,1.));
#7858=DIRECTION('center_axis',(0.,0.,1.));
#7859=DIRECTION('ref_axis',(1.,0.,0.));
#7860=DIRECTION('',(0.6,0.8,0.));
#7861=DIRECTION('',(0.,-1.,0.));
#7862=DIRECTION('',(1.,0.,0.));
#7863=DIRECTION('',(0.,1.,0.));
#7864=DIRECTION('',(-1.,0.,0.));
#7865=DIRECTION('center_axis',(0.,0.,1.));
#7866=DIRECTION('ref_axis',(-0.0955793180441842,0.995421817101779,0.));
#7867=DIRECTION('center_axis',(0.8,-0.6,0.));
#7868=DIRECTION('ref_axis',(0.6,0.8,0.));
#7869=DIRECTION('',(0.,0.,-1.));
#7870=DIRECTION('',(-0.6,-0.8,0.));
#7871=DIRECTION('center_axis',(0.,0.,1.));
#7872=DIRECTION('ref_axis',(4.44089209850063E-15,1.,0.));
#7873=DIRECTION('center_axis',(0.,0.,1.));
#7874=DIRECTION('ref_axis',(4.44089209850063E-15,1.,0.));
#7875=DIRECTION('center_axis',(0.,0.,1.));
#7876=DIRECTION('ref_axis',(4.44089209850063E-15,1.,0.));
#7877=DIRECTION('',(0.,0.,1.));
#7878=DIRECTION('center_axis',(0.,0.,1.));
#7879=DIRECTION('ref_axis',(-0.0955793180441842,0.995421817101779,0.));
#7880=DIRECTION('center_axis',(0.,0.,1.));
#7881=DIRECTION('ref_axis',(-0.0955793180441842,0.995421817101779,0.));
#7882=DIRECTION('',(0.,0.,1.));
#7883=DIRECTION('center_axis',(0.,0.,1.));
#7884=DIRECTION('ref_axis',(1.,0.,0.));
#7885=DIRECTION('',(0.,1.,0.));
#7886=DIRECTION('',(1.,0.,0.));
#7887=DIRECTION('center_axis',(-1.,0.,0.));
#7888=DIRECTION('ref_axis',(0.,-1.,0.));
#7889=DIRECTION('',(0.,0.,1.));
#7890=DIRECTION('',(0.,1.,0.));
#7891=DIRECTION('',(0.,0.,1.));
#7892=DIRECTION('center_axis',(0.,1.,0.));
#7893=DIRECTION('ref_axis',(-1.,0.,0.));
#7894=DIRECTION('',(0.,0.,1.));
#7895=DIRECTION('',(-1.,0.,0.));
#7896=DIRECTION('',(0.,0.,1.));
#7897=DIRECTION('',(1.,0.,0.));
#7898=DIRECTION('center_axis',(1.,0.,0.));
#7899=DIRECTION('ref_axis',(0.,1.,0.));
#7900=DIRECTION('',(0.,0.,1.));
#7901=DIRECTION('',(0.,-1.,0.));
#7902=DIRECTION('center_axis',(0.,0.,1.));
#7903=DIRECTION('ref_axis',(1.,0.,0.));
#7904=DIRECTION('center_axis',(0.,-1.,0.));
#7905=DIRECTION('ref_axis',(1.,0.,0.));
#7906=DIRECTION('',(-1.,0.,0.));
#7907=DIRECTION('',(0.,0.,-1.));
#7908=DIRECTION('',(1.,0.,0.));
#7909=DIRECTION('center_axis',(0.,0.,1.));
#7910=DIRECTION('ref_axis',(1.,0.,0.));
#7911=DIRECTION('',(0.,-1.,0.));
#7912=DIRECTION('center_axis',(0.,0.,1.));
#7913=DIRECTION('ref_axis',(1.,0.,0.));
#7914=DIRECTION('',(-0.447213595499958,-0.894427190999916,0.));
#7915=DIRECTION('',(-0.694594513699567,0.719401460617409,0.));
#7916=DIRECTION('center_axis',(0.,0.,1.));
#7917=DIRECTION('ref_axis',(1.,0.,0.));
#7918=DIRECTION('',(-0.694594513699567,0.719401460617409,0.));
#7919=DIRECTION('',(-1.,0.,0.));
#7920=DIRECTION('',(0.,1.,0.));
#7921=DIRECTION('',(1.,0.,0.));
#7922=DIRECTION('',(0.87524153543927,-0.483686111690123,0.));
#7923=DIRECTION('center_axis',(0.,0.,1.));
#7924=DIRECTION('ref_axis',(1.,0.,0.));
#7925=DIRECTION('',(0.87524153543927,-0.483686111690123,0.));
#7926=DIRECTION('center_axis',(0.,0.,1.));
#7927=DIRECTION('ref_axis',(1.,0.,0.));
#7928=DIRECTION('center_axis',(0.,0.,-1.));
#7929=DIRECTION('ref_axis',(-1.,2.01858731750028E-16,0.));
#7930=DIRECTION('center_axis',(1.,0.,0.));
#7931=DIRECTION('ref_axis',(0.,1.,0.));
#7932=DIRECTION('',(0.,0.,1.));
#7933=DIRECTION('',(0.,1.,0.));
#7934=DIRECTION('center_axis',(0.,0.,1.));
#7935=DIRECTION('ref_axis',(1.,0.,0.));
#7936=DIRECTION('',(0.,0.,1.));
#7937=DIRECTION('center_axis',(0.,0.,1.));
#7938=DIRECTION('ref_axis',(1.,0.,0.));
#7939=DIRECTION('center_axis',(0.,0.,1.));
#7940=DIRECTION('ref_axis',(1.,0.,0.));
#7941=DIRECTION('center_axis',(0.,0.,1.));
#7942=DIRECTION('ref_axis',(1.,0.,0.));
#7943=DIRECTION('',(0.,0.,-1.));
#7944=DIRECTION('center_axis',(0.,0.,1.));
#7945=DIRECTION('ref_axis',(1.,0.,0.));
#7946=DIRECTION('',(0.87524153543927,-0.483686111690123,0.));
#7947=DIRECTION('center_axis',(0.,0.,1.));
#7948=DIRECTION('ref_axis',(1.,0.,0.));
#7949=DIRECTION('',(0.87524153543927,-0.483686111690123,0.));
#7950=DIRECTION('',(1.,0.,0.));
#7951=DIRECTION('',(0.,1.,0.));
#7952=DIRECTION('',(-1.,0.,0.));
#7953=DIRECTION('',(-0.694594513699567,0.719401460617409,0.));
#7954=DIRECTION('center_axis',(0.,0.,1.));
#7955=DIRECTION('ref_axis',(1.,0.,0.));
#7956=DIRECTION('',(-0.694594513699567,0.719401460617409,0.));
#7957=DIRECTION('',(-0.447213595499958,-0.894427190999916,0.));
#7958=DIRECTION('center_axis',(0.,0.,1.));
#7959=DIRECTION('ref_axis',(-1.,0.,0.));
#7960=DIRECTION('center_axis',(0.,0.,1.));
#7961=DIRECTION('ref_axis',(1.,0.,0.));
#7962=DIRECTION('center_axis',(0.,-1.,0.));
#7963=DIRECTION('ref_axis',(-1.,0.,0.));
#7964=DIRECTION('center_axis',(0.,0.,1.));
#7965=DIRECTION('ref_axis',(-1.,2.01858731750028E-16,0.));
#7966=DIRECTION('center_axis',(0.,0.,-1.));
#7967=DIRECTION('ref_axis',(1.,0.,0.));
#7968=DIRECTION('center_axis',(0.,0.,-1.));
#7969=DIRECTION('ref_axis',(-1.,0.,0.));
#7970=DIRECTION('center_axis',(0.,0.,-1.));
#7971=DIRECTION('ref_axis',(-1.,0.,0.));
#7972=DIRECTION('',(0.,0.,-1.));
#7973=DIRECTION('center_axis',(0.,0.,-1.));
#7974=DIRECTION('ref_axis',(-1.,0.,0.));
#7975=DIRECTION('center_axis',(0.,-1.,0.));
#7976=DIRECTION('ref_axis',(1.,0.,0.));
#7977=DIRECTION('center_axis',(0.,0.,1.));
#7978=DIRECTION('ref_axis',(1.,0.,0.));
#7979=DIRECTION('',(0.,0.,-1.));
#7980=DIRECTION('',(0.,0.,1.));
#7981=DIRECTION('center_axis',(0.,0.,1.));
#7982=DIRECTION('ref_axis',(-0.483686111690122,-0.87524153543927,0.));
#7983=DIRECTION('',(0.,0.,1.));
#7984=DIRECTION('',(0.,0.,-1.));
#7985=DIRECTION('center_axis',(-0.483686111690123,-0.87524153543927,0.));
#7986=DIRECTION('ref_axis',(0.87524153543927,-0.483686111690123,0.));
#7987=DIRECTION('',(0.,0.,1.));
#7988=DIRECTION('center_axis',(0.719401460617409,0.694594513699567,0.));
#7989=DIRECTION('ref_axis',(-0.694594513699567,0.719401460617409,0.));
#7990=DIRECTION('',(0.,0.,1.));
#7991=DIRECTION('center_axis',(-0.483686111690123,-0.87524153543927,0.));
#7992=DIRECTION('ref_axis',(0.87524153543927,-0.483686111690123,0.));
#7993=DIRECTION('center_axis',(-0.894427190999916,0.447213595499958,0.));
#7994=DIRECTION('ref_axis',(-0.447213595499958,-0.894427190999916,0.));
#7995=DIRECTION('',(0.,0.,1.));
#7996=DIRECTION('center_axis',(0.719401460617409,0.694594513699567,0.));
#7997=DIRECTION('ref_axis',(-0.694594513699567,0.719401460617409,0.));
#7998=DIRECTION('center_axis',(0.,1.,0.));
#7999=DIRECTION('ref_axis',(-1.,0.,0.));
#8000=DIRECTION('',(0.,0.,1.));
#8001=DIRECTION('center_axis',(1.,0.,0.));
#8002=DIRECTION('ref_axis',(0.,1.,0.));
#8003=DIRECTION('',(0.,0.,1.));
#8004=DIRECTION('center_axis',(0.,-1.,0.));
#8005=DIRECTION('ref_axis',(1.,0.,0.));
#8006=DIRECTION('axis',(0.,0.,1.));
#8007=DIRECTION('refdir',(1.,0.,0.));
#8008=DIRECTION('center_axis',(0.,0.,-1.));
#8009=DIRECTION('ref_axis',(1.,0.,0.));
#8010=DIRECTION('center_axis',(0.,0.,-1.));
#8011=DIRECTION('ref_axis',(1.,0.,0.));
#8012=DIRECTION('',(0.,0.,-1.));
#8013=DIRECTION('center_axis',(0.,0.,1.));
#8014=DIRECTION('ref_axis',(1.,0.,0.));
#8015=DIRECTION('center_axis',(0.,0.,-1.));
#8016=DIRECTION('ref_axis',(1.,0.,0.));
#8017=DIRECTION('center_axis',(0.,0.,-1.));
#8018=DIRECTION('ref_axis',(1.,0.,0.));
#8019=DIRECTION('',(0.,0.,-1.));
#8020=DIRECTION('center_axis',(0.,0.,1.));
#8021=DIRECTION('ref_axis',(1.,0.,0.));
#8022=DIRECTION('center_axis',(0.,0.,-1.));
#8023=DIRECTION('ref_axis',(1.,0.,0.));
#8024=DIRECTION('center_axis',(0.,0.,-1.));
#8025=DIRECTION('ref_axis',(1.,0.,0.));
#8026=DIRECTION('',(0.,0.,-1.));
#8027=DIRECTION('center_axis',(0.,0.,1.));
#8028=DIRECTION('ref_axis',(1.,0.,0.));
#8029=DIRECTION('center_axis',(1.,0.,0.));
#8030=DIRECTION('ref_axis',(0.,0.,-1.));
#8031=DIRECTION('',(0.,-1.,0.));
#8032=DIRECTION('',(0.,0.8,0.6));
#8033=DIRECTION('',(0.,0.,1.));
#8034=DIRECTION('center_axis',(0.,0.6,-0.8));
#8035=DIRECTION('ref_axis',(0.,0.8,0.6));
#8036=DIRECTION('',(0.,0.8,0.6));
#8037=DIRECTION('',(-1.,0.,0.));
#8038=DIRECTION('',(1.,0.,0.));
#8039=DIRECTION('center_axis',(1.,0.,0.));
#8040=DIRECTION('ref_axis',(0.,2.22044604925031E-16,1.));
#8041=DIRECTION('',(0.,1.,0.));
#8042=DIRECTION('',(0.,0.,1.));
#8043=DIRECTION('center_axis',(0.,0.,1.));
#8044=DIRECTION('ref_axis',(1.,0.,0.));
#8045=DIRECTION('',(0.6,0.8,0.));
#8046=DIRECTION('',(0.,-1.,0.));
#8047=DIRECTION('',(-1.,0.,0.));
#8048=DIRECTION('center_axis',(0.,0.,1.));
#8049=DIRECTION('ref_axis',(-0.0955793180441842,0.995421817101779,0.));
#8050=DIRECTION('center_axis',(0.,0.,1.));
#8051=DIRECTION('ref_axis',(1.,0.,0.));
#8052=DIRECTION('center_axis',(0.,0.,1.));
#8053=DIRECTION('ref_axis',(4.44089209850063E-15,1.,0.));
#8054=DIRECTION('center_axis',(0.8,-0.6,0.));
#8055=DIRECTION('ref_axis',(0.6,0.8,0.));
#8056=DIRECTION('',(0.,0.,-1.));
#8057=DIRECTION('',(-0.6,-0.8,0.));
#8058=DIRECTION('center_axis',(0.,0.,1.));
#8059=DIRECTION('ref_axis',(4.44089209850063E-15,1.,0.));
#8060=DIRECTION('center_axis',(0.,0.,1.));
#8061=DIRECTION('ref_axis',(4.44089209850063E-15,1.,0.));
#8062=DIRECTION('',(0.,0.,1.));
#8063=DIRECTION('center_axis',(0.,0.,1.));
#8064=DIRECTION('ref_axis',(-0.0955793180441842,0.995421817101779,0.));
#8065=DIRECTION('center_axis',(0.,0.,1.));
#8066=DIRECTION('ref_axis',(-0.0955793180441842,0.995421817101779,0.));
#8067=DIRECTION('',(0.,0.,1.));
#8068=DIRECTION('center_axis',(0.,0.,1.));
#8069=DIRECTION('ref_axis',(1.,0.,0.));
#8070=DIRECTION('',(0.,-1.,0.));
#8071=DIRECTION('',(-1.,0.,0.));
#8072=DIRECTION('',(0.,1.,0.));
#8073=DIRECTION('',(1.,0.,0.));
#8074=DIRECTION('center_axis',(1.,0.,0.));
#8075=DIRECTION('ref_axis',(0.,1.,0.));
#8076=DIRECTION('',(0.,0.,1.));
#8077=DIRECTION('',(0.,1.,0.));
#8078=DIRECTION('',(0.,0.,1.));
#8079=DIRECTION('center_axis',(0.,-1.,0.));
#8080=DIRECTION('ref_axis',(1.,0.,0.));
#8081=DIRECTION('',(-1.,0.,0.));
#8082=DIRECTION('',(0.,0.,-1.));
#8083=DIRECTION('',(1.,0.,0.));
#8084=DIRECTION('',(0.,0.,1.));
#8085=DIRECTION('center_axis',(0.,0.,1.));
#8086=DIRECTION('ref_axis',(1.,0.,0.));
#8087=DIRECTION('',(1.,0.,0.));
#8088=DIRECTION('',(0.,-1.,0.));
#8089=DIRECTION('center_axis',(0.,0.,1.));
#8090=DIRECTION('ref_axis',(1.,0.,0.));
#8091=DIRECTION('',(-0.447213595499958,-0.894427190999916,0.));
#8092=DIRECTION('',(-0.694594513699567,0.719401460617409,0.));
#8093=DIRECTION('center_axis',(0.,0.,1.));
#8094=DIRECTION('ref_axis',(1.,0.,0.));
#8095=DIRECTION('',(-0.694594513699567,0.719401460617409,0.));
#8096=DIRECTION('',(-1.,0.,0.));
#8097=DIRECTION('',(0.,1.,0.));
#8098=DIRECTION('',(1.,0.,0.));
#8099=DIRECTION('',(0.87524153543927,-0.483686111690123,0.));
#8100=DIRECTION('center_axis',(0.,0.,1.));
#8101=DIRECTION('ref_axis',(1.,0.,0.));
#8102=DIRECTION('',(0.87524153543927,-0.483686111690123,0.));
#8103=DIRECTION('center_axis',(0.,0.,1.));
#8104=DIRECTION('ref_axis',(1.,0.,0.));
#8105=DIRECTION('center_axis',(0.,0.,-1.));
#8106=DIRECTION('ref_axis',(-1.,2.01858731750028E-16,0.));
#8107=DIRECTION('center_axis',(0.,1.,0.));
#8108=DIRECTION('ref_axis',(-1.,0.,0.));
#8109=DIRECTION('',(0.,0.,1.));
#8110=DIRECTION('',(-1.,0.,0.));
#8111=DIRECTION('',(0.,0.,1.));
#8112=DIRECTION('center_axis',(-1.,0.,0.));
#8113=DIRECTION('ref_axis',(0.,-1.,0.));
#8114=DIRECTION('',(0.,-1.,0.));
#8115=DIRECTION('center_axis',(1.,0.,0.));
#8116=DIRECTION('ref_axis',(0.,1.,0.));
#8117=DIRECTION('',(0.,0.,1.));
#8118=DIRECTION('',(0.,1.,0.));
#8119=DIRECTION('center_axis',(0.,0.,1.));
#8120=DIRECTION('ref_axis',(1.,0.,0.));
#8121=DIRECTION('',(0.,0.,1.));
#8122=DIRECTION('center_axis',(0.,0.,1.));
#8123=DIRECTION('ref_axis',(1.,0.,0.));
#8124=DIRECTION('center_axis',(0.,0.,1.));
#8125=DIRECTION('ref_axis',(1.,0.,0.));
#8126=DIRECTION('center_axis',(0.,0.,1.));
#8127=DIRECTION('ref_axis',(1.,0.,0.));
#8128=DIRECTION('',(0.,0.,-1.));
#8129=DIRECTION('center_axis',(0.,0.,1.));
#8130=DIRECTION('ref_axis',(1.,0.,0.));
#8131=DIRECTION('',(0.87524153543927,-0.483686111690123,0.));
#8132=DIRECTION('center_axis',(0.,0.,1.));
#8133=DIRECTION('ref_axis',(1.,0.,0.));
#8134=DIRECTION('',(0.87524153543927,-0.483686111690123,0.));
#8135=DIRECTION('',(1.,0.,0.));
#8136=DIRECTION('',(0.,1.,0.));
#8137=DIRECTION('',(-1.,0.,0.));
#8138=DIRECTION('',(-0.694594513699567,0.719401460617409,0.));
#8139=DIRECTION('center_axis',(0.,0.,1.));
#8140=DIRECTION('ref_axis',(1.,0.,0.));
#8141=DIRECTION('',(-0.694594513699567,0.719401460617409,0.));
#8142=DIRECTION('',(-0.447213595499958,-0.894427190999916,0.));
#8143=DIRECTION('center_axis',(0.,0.,1.));
#8144=DIRECTION('ref_axis',(-1.,0.,0.));
#8145=DIRECTION('center_axis',(0.,0.,1.));
#8146=DIRECTION('ref_axis',(1.,0.,0.));
#8147=DIRECTION('center_axis',(0.,-1.,0.));
#8148=DIRECTION('ref_axis',(-1.,0.,0.));
#8149=DIRECTION('center_axis',(0.,0.,1.));
#8150=DIRECTION('ref_axis',(-1.,2.01858731750028E-16,0.));
#8151=DIRECTION('center_axis',(0.,0.,-1.));
#8152=DIRECTION('ref_axis',(1.,0.,0.));
#8153=DIRECTION('center_axis',(0.,0.,-1.));
#8154=DIRECTION('ref_axis',(-1.,0.,0.));
#8155=DIRECTION('center_axis',(0.,0.,-1.));
#8156=DIRECTION('ref_axis',(-1.,0.,0.));
#8157=DIRECTION('',(0.,0.,-1.));
#8158=DIRECTION('center_axis',(0.,0.,-1.));
#8159=DIRECTION('ref_axis',(-1.,0.,0.));
#8160=DIRECTION('center_axis',(0.,-1.,0.));
#8161=DIRECTION('ref_axis',(1.,0.,0.));
#8162=DIRECTION('center_axis',(0.,0.,1.));
#8163=DIRECTION('ref_axis',(1.,0.,0.));
#8164=DIRECTION('',(0.,0.,-1.));
#8165=DIRECTION('',(0.,0.,1.));
#8166=DIRECTION('center_axis',(0.,0.,1.));
#8167=DIRECTION('ref_axis',(-0.483686111690122,-0.87524153543927,0.));
#8168=DIRECTION('',(0.,0.,1.));
#8169=DIRECTION('',(0.,0.,-1.));
#8170=DIRECTION('center_axis',(-0.483686111690123,-0.87524153543927,0.));
#8171=DIRECTION('ref_axis',(0.87524153543927,-0.483686111690123,0.));
#8172=DIRECTION('',(0.,0.,1.));
#8173=DIRECTION('center_axis',(0.719401460617409,0.694594513699567,0.));
#8174=DIRECTION('ref_axis',(-0.694594513699567,0.719401460617409,0.));
#8175=DIRECTION('',(0.,0.,1.));
#8176=DIRECTION('center_axis',(-0.483686111690123,-0.87524153543927,0.));
#8177=DIRECTION('ref_axis',(0.87524153543927,-0.483686111690123,0.));
#8178=DIRECTION('center_axis',(-0.894427190999916,0.447213595499958,0.));
#8179=DIRECTION('ref_axis',(-0.447213595499958,-0.894427190999916,0.));
#8180=DIRECTION('',(0.,0.,1.));
#8181=DIRECTION('center_axis',(0.719401460617409,0.694594513699567,0.));
#8182=DIRECTION('ref_axis',(-0.694594513699567,0.719401460617409,0.));
#8183=DIRECTION('center_axis',(0.,1.,0.));
#8184=DIRECTION('ref_axis',(-1.,0.,0.));
#8185=DIRECTION('',(0.,0.,1.));
#8186=DIRECTION('center_axis',(1.,0.,0.));
#8187=DIRECTION('ref_axis',(0.,1.,0.));
#8188=DIRECTION('',(0.,0.,1.));
#8189=DIRECTION('center_axis',(0.,-1.,0.));
#8190=DIRECTION('ref_axis',(1.,0.,0.));
#8191=DIRECTION('axis',(0.,0.,1.));
#8192=DIRECTION('refdir',(1.,0.,0.));
#8193=DIRECTION('center_axis',(0.,0.,1.));
#8194=DIRECTION('ref_axis',(1.,0.,0.));
#8195=DIRECTION('center_axis',(0.,0.,1.));
#8196=DIRECTION('ref_axis',(1.,0.,0.));
#8197=DIRECTION('',(0.,0.,1.));
#8198=DIRECTION('center_axis',(0.,0.,1.));
#8199=DIRECTION('ref_axis',(1.,0.,0.));
#8200=DIRECTION('center_axis',(0.,0.,-1.));
#8201=DIRECTION('ref_axis',(-1.,0.,0.));
#8202=DIRECTION('center_axis',(0.,0.,-1.));
#8203=DIRECTION('ref_axis',(1.,0.,0.));
#8204=DIRECTION('center_axis',(0.,0.,1.));
#8205=DIRECTION('ref_axis',(1.,0.,0.));
#8206=DIRECTION('center_axis',(0.,0.,1.));
#8207=DIRECTION('ref_axis',(1.,0.,0.));
#8208=DIRECTION('center_axis',(0.,0.,1.));
#8209=DIRECTION('ref_axis',(1.,0.,0.));
#8210=DIRECTION('center_axis',(0.,0.,1.));
#8211=DIRECTION('ref_axis',(1.,0.,0.));
#8212=DIRECTION('',(0.,0.,-1.));
#8213=DIRECTION('center_axis',(0.,0.,1.));
#8214=DIRECTION('ref_axis',(1.,0.,0.));
#8215=DIRECTION('center_axis',(0.,0.,1.));
#8216=DIRECTION('ref_axis',(1.,0.,0.));
#8217=DIRECTION('center_axis',(0.,0.,1.));
#8218=DIRECTION('ref_axis',(1.,0.,0.));
#8219=DIRECTION('center_axis',(0.,0.,1.));
#8220=DIRECTION('ref_axis',(1.,0.,0.));
#8221=DIRECTION('',(0.,0.,-1.));
#8222=DIRECTION('center_axis',(0.,0.,1.));
#8223=DIRECTION('ref_axis',(1.,0.,0.));
#8224=DIRECTION('center_axis',(0.,0.,1.));
#8225=DIRECTION('ref_axis',(1.,0.,0.));
#8226=DIRECTION('center_axis',(0.,0.,1.));
#8227=DIRECTION('ref_axis',(1.,0.,0.));
#8228=DIRECTION('',(0.,0.,-1.));
#8229=DIRECTION('center_axis',(0.,0.,1.));
#8230=DIRECTION('ref_axis',(1.,0.,0.));
#8231=DIRECTION('axis',(0.,0.,1.));
#8232=DIRECTION('refdir',(1.,0.,0.));
#8233=DIRECTION('center_axis',(-1.,0.,0.));
#8234=DIRECTION('ref_axis',(0.,1.,0.));
#8235=DIRECTION('',(0.,0.,1.));
#8236=DIRECTION('',(0.,-1.,0.));
#8237=DIRECTION('',(0.,0.,-1.));
#8238=DIRECTION('',(0.,1.,0.));
#8239=DIRECTION('center_axis',(1.,0.,0.));
#8240=DIRECTION('ref_axis',(0.,-1.,0.));
#8241=DIRECTION('',(0.,0.,-1.));
#8242=DIRECTION('',(0.,-1.,0.));
#8243=DIRECTION('',(0.,0.,1.));
#8244=DIRECTION('',(0.,1.,0.));
#8245=DIRECTION('center_axis',(0.,0.,1.));
#8246=DIRECTION('ref_axis',(1.,0.,0.));
#8247=DIRECTION('center_axis',(0.,0.,1.));
#8248=DIRECTION('ref_axis',(1.,0.,0.));
#8249=DIRECTION('center_axis',(0.,0.,-1.));
#8250=DIRECTION('ref_axis',(1.,0.,0.));
#8251=DIRECTION('center_axis',(0.,0.,1.));
#8252=DIRECTION('ref_axis',(6.12323399573677E-17,-1.,0.));
#8253=DIRECTION('center_axis',(0.,0.,-1.));
#8254=DIRECTION('ref_axis',(1.,0.,0.));
#8255=DIRECTION('center_axis',(0.,0.,1.));
#8256=DIRECTION('ref_axis',(6.12323399573677E-17,-1.,0.));
#8257=DIRECTION('center_axis',(0.,0.,1.));
#8258=DIRECTION('ref_axis',(1.,0.,0.));
#8259=DIRECTION('center_axis',(0.,0.,1.));
#8260=DIRECTION('ref_axis',(1.,0.,0.));
#8261=DIRECTION('axis',(0.,0.,1.));
#8262=DIRECTION('refdir',(1.,0.,0.));
#8263=DIRECTION('axis',(0.,0.,1.));
#8264=DIRECTION('refdir',(1.,0.,0.));
#8265=DIRECTION('center_axis',(0.,0.,-1.));
#8266=DIRECTION('ref_axis',(1.,0.,0.));
#8267=DIRECTION('center_axis',(1.01338750660366E-31,-1.26069923670246E-19,
-1.));
#8268=DIRECTION('ref_axis',(1.,0.,0.));
#8269=DIRECTION('',(0.,0.,-1.));
#8270=DIRECTION('center_axis',(-1.01338750660366E-31,1.26069923670246E-19,
1.));
#8271=DIRECTION('ref_axis',(1.,0.,0.));
#8272=DIRECTION('center_axis',(0.,0.,-1.));
#8273=DIRECTION('ref_axis',(1.,0.,0.));
#8274=DIRECTION('center_axis',(1.01338750660366E-31,-1.26069923670246E-19,
-1.));
#8275=DIRECTION('ref_axis',(1.,0.,0.));
#8276=DIRECTION('',(0.,0.,-1.));
#8277=DIRECTION('center_axis',(-1.01338750660366E-31,1.26069923670246E-19,
1.));
#8278=DIRECTION('ref_axis',(1.,0.,0.));
#8279=DIRECTION('center_axis',(0.,0.,-1.));
#8280=DIRECTION('ref_axis',(1.,0.,0.));
#8281=DIRECTION('center_axis',(1.01338750660366E-31,-1.26069923670246E-19,
-1.));
#8282=DIRECTION('ref_axis',(1.,0.,0.));
#8283=DIRECTION('',(0.,0.,-1.));
#8284=DIRECTION('center_axis',(-1.01338750660366E-31,1.26069923670246E-19,
1.));
#8285=DIRECTION('ref_axis',(1.,0.,0.));
#8286=DIRECTION('center_axis',(0.,0.,-1.));
#8287=DIRECTION('ref_axis',(1.,0.,0.));
#8288=DIRECTION('center_axis',(1.01338750660366E-31,-1.26069923670246E-19,
-1.));
#8289=DIRECTION('ref_axis',(1.,0.,0.));
#8290=DIRECTION('',(0.,0.,-1.));
#8291=DIRECTION('center_axis',(-1.01338750660366E-31,1.26069923670246E-19,
1.));
#8292=DIRECTION('ref_axis',(1.,0.,0.));
#8293=DIRECTION('center_axis',(0.,0.,-1.));
#8294=DIRECTION('ref_axis',(1.,0.,0.));
#8295=DIRECTION('center_axis',(1.01338750660366E-31,-1.26069923670246E-19,
-1.));
#8296=DIRECTION('ref_axis',(1.,0.,0.));
#8297=DIRECTION('',(0.,0.,-1.));
#8298=DIRECTION('center_axis',(0.,0.,-1.));
#8299=DIRECTION('ref_axis',(1.,0.,0.));
#8300=DIRECTION('center_axis',(0.,0.,-1.));
#8301=DIRECTION('ref_axis',(1.,0.,0.));
#8302=DIRECTION('center_axis',(0.,0.,1.));
#8303=DIRECTION('ref_axis',(1.,0.,0.));
#8304=DIRECTION('center_axis',(0.,0.,-1.));
#8305=DIRECTION('ref_axis',(1.,0.,0.));
#8306=DIRECTION('center_axis',(1.01338750660366E-31,-1.26069923670246E-19,
-1.));
#8307=DIRECTION('ref_axis',(1.,0.,0.));
#8308=DIRECTION('',(0.,0.,-1.));
#8309=DIRECTION('center_axis',(0.,0.,-1.));
#8310=DIRECTION('ref_axis',(1.,0.,0.));
#8311=DIRECTION('center_axis',(0.,0.,-1.));
#8312=DIRECTION('ref_axis',(1.,0.,0.));
#8313=DIRECTION('center_axis',(0.,0.,1.));
#8314=DIRECTION('ref_axis',(1.,0.,0.));
#8315=DIRECTION('center_axis',(0.,0.,-1.));
#8316=DIRECTION('ref_axis',(1.,0.,0.));
#8317=DIRECTION('',(0.,0.,-1.));
#8318=DIRECTION('center_axis',(0.,0.,1.));
#8319=DIRECTION('ref_axis',(1.,0.,0.));
#8320=DIRECTION('center_axis',(0.,0.,-1.));
#8321=DIRECTION('ref_axis',(1.,0.,0.));
#8322=DIRECTION('',(0.,0.,-1.));
#8323=DIRECTION('center_axis',(0.,0.,1.));
#8324=DIRECTION('ref_axis',(1.,0.,0.));
#8325=DIRECTION('center_axis',(0.,-1.,0.));
#8326=DIRECTION('ref_axis',(-1.,0.,0.));
#8327=DIRECTION('',(0.0523359562429438,0.,0.998629534754574));
#8328=DIRECTION('',(1.,0.,0.));
#8329=DIRECTION('',(-0.0523359562429438,0.,-0.998629534754574));
#8330=DIRECTION('',(1.,0.,0.));
#8331=DIRECTION('center_axis',(0.,-1.,0.));
#8332=DIRECTION('ref_axis',(-1.,0.,0.));
#8333=DIRECTION('',(0.,0.,-1.));
#8334=DIRECTION('',(1.,0.,0.));
#8335=DIRECTION('',(0.,0.,1.));
#8336=DIRECTION('',(1.,0.,0.));
#8337=DIRECTION('center_axis',(0.,-1.,0.));
#8338=DIRECTION('ref_axis',(-1.,0.,0.));
#8339=DIRECTION('',(0.,0.,-1.));
#8340=DIRECTION('',(1.,0.,0.));
#8341=DIRECTION('',(0.,0.,1.));
#8342=DIRECTION('',(1.,0.,0.));
#8343=DIRECTION('center_axis',(0.,-1.,0.));
#8344=DIRECTION('ref_axis',(-1.,0.,0.));
#8345=DIRECTION('',(0.,0.,-1.));
#8346=DIRECTION('',(1.,0.,0.));
#8347=DIRECTION('',(0.,0.,1.));
#8348=DIRECTION('',(1.,0.,0.));
#8349=DIRECTION('center_axis',(0.,1.,0.));
#8350=DIRECTION('ref_axis',(1.,0.,0.));
#8351=DIRECTION('',(-0.0523359562429438,0.,-0.998629534754574));
#8352=DIRECTION('',(-1.,0.,0.));
#8353=DIRECTION('',(0.0523359562429438,0.,0.998629534754574));
#8354=DIRECTION('',(-1.,0.,0.));
#8355=DIRECTION('center_axis',(0.,1.,0.));
#8356=DIRECTION('ref_axis',(1.,0.,0.));
#8357=DIRECTION('',(0.,0.,1.));
#8358=DIRECTION('',(-1.,0.,0.));
#8359=DIRECTION('',(0.,0.,-1.));
#8360=DIRECTION('',(-1.,0.,0.));
#8361=DIRECTION('center_axis',(0.,1.,0.));
#8362=DIRECTION('ref_axis',(1.,0.,0.));
#8363=DIRECTION('',(0.,0.,1.));
#8364=DIRECTION('',(-1.,0.,0.));
#8365=DIRECTION('',(0.,0.,-1.));
#8366=DIRECTION('',(-1.,0.,0.));
#8367=DIRECTION('center_axis',(0.,0.,1.));
#8368=DIRECTION('ref_axis',(1.,0.,0.));
#8369=DIRECTION('center_axis',(0.,0.,1.));
#8370=DIRECTION('ref_axis',(1.,0.,0.));
#8371=DIRECTION('center_axis',(0.,0.,1.));
#8372=DIRECTION('ref_axis',(1.,0.,0.));
#8373=DIRECTION('center_axis',(0.,0.,1.));
#8374=DIRECTION('ref_axis',(1.,0.,0.));
#8375=DIRECTION('center_axis',(0.,0.,1.));
#8376=DIRECTION('ref_axis',(1.,0.,0.));
#8377=DIRECTION('',(0.,1.,0.));
#8378=DIRECTION('',(0.,-1.,0.));
#8379=DIRECTION('center_axis',(0.,0.,1.));
#8380=DIRECTION('ref_axis',(1.,0.,0.));
#8381=DIRECTION('',(0.,-1.,0.));
#8382=DIRECTION('',(0.,1.,0.));
#8383=DIRECTION('center_axis',(0.,0.,1.));
#8384=DIRECTION('ref_axis',(1.,0.,0.));
#8385=DIRECTION('',(0.,-1.,0.));
#8386=DIRECTION('',(0.,1.,0.));
#8387=DIRECTION('center_axis',(0.,0.,1.));
#8388=DIRECTION('ref_axis',(1.,0.,0.));
#8389=DIRECTION('',(0.,-1.,0.));
#8390=DIRECTION('',(-1.,0.,0.));
#8391=DIRECTION('',(0.,1.,0.));
#8392=DIRECTION('center_axis',(0.,1.,0.));
#8393=DIRECTION('ref_axis',(1.,0.,0.));
#8394=DIRECTION('',(0.,0.,1.));
#8395=DIRECTION('',(-1.,0.,0.));
#8396=DIRECTION('',(0.,0.,-1.));
#8397=DIRECTION('center_axis',(-1.,0.,0.));
#8398=DIRECTION('ref_axis',(0.,-1.,0.));
#8399=DIRECTION('',(0.,-1.,0.));
#8400=DIRECTION('',(0.,-1.,1.26069923670246E-19));
#8401=DIRECTION('center_axis',(1.,0.,0.));
#8402=DIRECTION('ref_axis',(0.,1.,0.));
#8403=DIRECTION('',(0.,1.,0.));
#8404=DIRECTION('',(0.,1.,-1.26069923670246E-19));
#8405=DIRECTION('',(0.,1.,0.));
#8406=DIRECTION('center_axis',(1.,0.,0.));
#8407=DIRECTION('ref_axis',(0.,1.,0.));
#8408=DIRECTION('',(0.,1.,0.));
#8409=DIRECTION('',(0.,1.,-1.26069923670246E-19));
#8410=DIRECTION('',(0.,1.,0.));
#8411=DIRECTION('center_axis',(1.,0.,0.));
#8412=DIRECTION('ref_axis',(0.,1.,0.));
#8413=DIRECTION('',(0.,1.,0.));
#8414=DIRECTION('',(0.,1.,-1.26069923670246E-19));
#8415=DIRECTION('',(0.,1.,0.));
#8416=DIRECTION('center_axis',(0.998629534754574,0.,-0.0523359562429438));
#8417=DIRECTION('ref_axis',(-0.0523359562429438,0.,-0.998629534754574));
#8418=DIRECTION('',(0.,-1.,0.));
#8419=DIRECTION('',(6.6070447339401E-21,-1.,1.26069923670246E-19));
#8420=DIRECTION('',(0.,-1.,0.));
#8421=DIRECTION('center_axis',(0.,0.,1.));
#8422=DIRECTION('ref_axis',(1.,0.,0.));
#8423=DIRECTION('',(0.,-1.,0.));
#8424=DIRECTION('',(0.,-1.,0.));
#8425=DIRECTION('',(0.,-1.,0.));
#8426=DIRECTION('',(0.,1.,0.));
#8427=DIRECTION('',(0.,-1.,0.));
#8428=DIRECTION('',(0.,1.,0.));
#8429=DIRECTION('',(0.,-1.,0.));
#8430=DIRECTION('',(0.,-1.,0.));
#8431=DIRECTION('',(0.,-1.,0.));
#8432=DIRECTION('',(0.,1.,0.));
#8433=DIRECTION('',(0.,1.,0.));
#8434=DIRECTION('center_axis',(0.,0.,1.));
#8435=DIRECTION('ref_axis',(1.,0.,0.));
#8436=DIRECTION('center_axis',(-1.01338750660366E-31,1.26069923670246E-19,
1.));
#8437=DIRECTION('ref_axis',(1.,0.,0.));
#8438=DIRECTION('',(0.,0.,-1.));
#8439=DIRECTION('center_axis',(0.,0.,1.));
#8440=DIRECTION('ref_axis',(1.,0.,0.));
#8441=DIRECTION('center_axis',(-1.01338750660366E-31,1.26069923670246E-19,
1.));
#8442=DIRECTION('ref_axis',(1.,0.,0.));
#8443=DIRECTION('',(0.,0.,-1.));
#8444=DIRECTION('center_axis',(1.,0.,0.));
#8445=DIRECTION('ref_axis',(0.,1.,0.));
#8446=DIRECTION('',(0.,1.,-1.26069923670246E-19));
#8447=DIRECTION('center_axis',(0.995216631131787,0.0976926666577189,1.18580395612125E-14));
#8448=DIRECTION('ref_axis',(0.0975341006448478,-0.993601284365854,0.0569524970297685));
#8449=DIRECTION('center_axis',(-1.01338750660366E-31,1.26069923670246E-19,
1.));
#8450=DIRECTION('ref_axis',(1.,0.,1.01338750660366E-31));
#8451=DIRECTION('center_axis',(-1.01338750660366E-31,1.26069923670246E-19,
1.));
#8452=DIRECTION('ref_axis',(1.,0.,1.01338750660366E-31));
#8453=DIRECTION('',(-6.60704473394009E-21,-1.,1.26069923670246E-19));
#8454=DIRECTION('center_axis',(-1.,0.,0.));
#8455=DIRECTION('ref_axis',(0.,-1.,0.));
#8456=DIRECTION('',(0.,-1.,1.26069923670246E-19));
#8457=DIRECTION('center_axis',(-1.01338750660366E-31,1.26069923670246E-19,
1.));
#8458=DIRECTION('ref_axis',(1.,0.,1.01338750660366E-31));
#8459=DIRECTION('center_axis',(-1.,0.,0.));
#8460=DIRECTION('ref_axis',(0.,-1.,0.));
#8461=DIRECTION('',(0.,-1.,1.26069923670246E-19));
#8462=DIRECTION('center_axis',(-1.01338750660366E-31,1.26069923670246E-19,
1.));
#8463=DIRECTION('ref_axis',(1.,0.,1.01338750660366E-31));
#8464=DIRECTION('center_axis',(-1.,0.,0.));
#8465=DIRECTION('ref_axis',(0.,-1.,0.));
#8466=DIRECTION('',(0.,-1.,1.26069923670246E-19));
#8467=DIRECTION('center_axis',(-0.982258063247475,0.187534256031586,1.45403402392141E-15));
#8468=DIRECTION('ref_axis',(1.48029736616688E-15,0.,1.));
#8469=DIRECTION('center_axis',(-1.01338750660366E-31,1.26069923670246E-19,
1.));
#8470=DIRECTION('ref_axis',(1.,0.,1.01338750660366E-31));
#8471=DIRECTION('',(-6.6070447339401E-21,1.,-1.26069923670246E-19));
#8472=DIRECTION('center_axis',(-0.982258063247479,-0.187534256031562,9.14061384143289E-15));
#8473=DIRECTION('ref_axis',(-0.187187393251729,0.980441281772238,0.0607928680392112));
#8474=DIRECTION('center_axis',(-0.45173408531537,0.373496730537872,-0.810207694632559));
#8475=DIRECTION('ref_axis',(-0.624418441188311,0.516273298501642,0.586142893463867));
#8476=DIRECTION('center_axis',(-2.96465769266614E-15,1.,0.));
#8477=DIRECTION('ref_axis',(0.,0.,1.));
#8478=DIRECTION('center_axis',(0.0522655346583812,-0.0518587053130894,0.997285810873755));
#8479=DIRECTION('ref_axis',(-0.998629534754574,0.,0.0523359562429445));
#8480=DIRECTION('center_axis',(0.377681861983732,-0.843372107574977,0.38220400219391));
#8481=DIRECTION('ref_axis',(0.592794689304902,0.537329962094562,0.599892463836113));
#8482=DIRECTION('center_axis',(0.995216631131786,-0.0976926666577302,0.));
#8483=DIRECTION('ref_axis',(0.,0.,1.));
#8484=DIRECTION('center_axis',(-0.0522650609395843,-0.052032719242908,0.997276771780618));
#8485=DIRECTION('ref_axis',(0.0975341006448596,0.993601284365853,0.0569524970297681));
#8486=DIRECTION('center_axis',(1.55158195278682E-16,1.,-2.96059473233375E-15));
#8487=DIRECTION('ref_axis',(0.998629534754574,0.,0.0523359562429438));
#8488=DIRECTION('center_axis',(-0.45173408531537,-0.373496730537869,-0.810207694632561));
#8489=DIRECTION('ref_axis',(-0.624418441188315,-0.516273298501641,0.586142893463864));
#8490=DIRECTION('center_axis',(0.0522655346583823,0.0518587053130918,0.997285810873755));
#8491=DIRECTION('ref_axis',(-0.187187393251729,-0.980441281772238,0.0607928680392122));
#8492=DIRECTION('center_axis',(-2.71526841737693E-16,-1.,-5.18104078158406E-15));
#8493=DIRECTION('ref_axis',(-0.998629534754574,0.,0.0523359562429439));
#8494=DIRECTION('center_axis',(-6.6070447339401E-21,1.,-1.26069923670246E-19));
#8495=DIRECTION('ref_axis',(-0.688354575693753,0.,0.725374371012289));
#8496=DIRECTION('center_axis',(-0.377681861983722,-0.843372107574983,-0.382204002193908));
#8497=DIRECTION('ref_axis',(0.592794689304909,-0.537329962094554,0.599892463836112));
#8498=DIRECTION('center_axis',(-0.0522650609395818,0.0520327192429072,0.997276771780618));
#8499=DIRECTION('ref_axis',(0.998629534754574,0.,0.0523359562429431));
#8500=DIRECTION('center_axis',(2.96465769266612E-15,-1.,0.));
#8501=DIRECTION('ref_axis',(0.,0.,1.));
#8502=DIRECTION('center_axis',(-6.60704473394009E-21,-1.,1.26069923670246E-19));
#8503=DIRECTION('ref_axis',(0.688354575693758,0.,0.725374371012284));
#8504=DIRECTION('',(6.60704473394009E-21,1.,-1.26069923670246E-19));
#8505=DIRECTION('center_axis',(-0.998629534754574,0.,-0.0523359562429438));
#8506=DIRECTION('ref_axis',(-0.0523359562429438,0.,0.998629534754574));
#8507=DIRECTION('center_axis',(-0.45173408531537,0.373496730537872,-0.81020769463256));
#8508=DIRECTION('ref_axis',(-0.624418441188311,0.516273298501643,0.586142893463866));
#8509=DIRECTION('center_axis',(-2.96465769266614E-15,1.,0.));
#8510=DIRECTION('ref_axis',(0.,0.,1.));
#8511=DIRECTION('center_axis',(-0.982258063247479,-0.187534256031562,9.14061384143289E-15));
#8512=DIRECTION('ref_axis',(-0.187187393251729,0.980441281772238,0.0607928680392111));
#8513=DIRECTION('center_axis',(0.0522655346583812,-0.0518587053130894,0.997285810873755));
#8514=DIRECTION('ref_axis',(-0.998629534754574,0.,0.0523359562429445));
#8515=DIRECTION('center_axis',(0.377681861983731,-0.843372107574978,0.38220400219391));
#8516=DIRECTION('ref_axis',(0.592794689304906,0.537329962094559,0.599892463836111));
#8517=DIRECTION('center_axis',(0.995216631131786,-0.0976926666577302,0.));
#8518=DIRECTION('ref_axis',(0.,0.,1.));
#8519=DIRECTION('center_axis',(1.55158195278682E-16,1.,-2.96059473233375E-15));
#8520=DIRECTION('ref_axis',(0.998629534754574,0.,0.0523359562429438));
#8521=DIRECTION('center_axis',(-0.0522650609395843,-0.052032719242908,0.997276771780618));
#8522=DIRECTION('ref_axis',(0.0975341006448596,0.993601284365853,0.0569524970297681));
#8523=DIRECTION('center_axis',(-0.45173408531537,-0.373496730537868,-0.810207694632561));
#8524=DIRECTION('ref_axis',(-0.624418441188315,-0.516273298501641,0.586142893463864));
#8525=DIRECTION('center_axis',(-0.982258063247475,0.187534256031586,1.45403402392141E-15));
#8526=DIRECTION('ref_axis',(1.48029736616688E-15,0.,1.));
#8527=DIRECTION('center_axis',(-2.71526841737693E-16,-1.,-5.18104078158406E-15));
#8528=DIRECTION('ref_axis',(-0.998629534754574,0.,0.0523359562429439));
#8529=DIRECTION('center_axis',(0.0522655346583823,0.0518587053130918,0.997285810873755));
#8530=DIRECTION('ref_axis',(-0.187187393251729,-0.980441281772238,0.0607928680392122));
#8531=DIRECTION('center_axis',(-6.6070447339401E-21,1.,-1.26069923670246E-19));
#8532=DIRECTION('ref_axis',(-0.688354575693753,0.,0.725374371012289));
#8533=DIRECTION('',(6.6070447339401E-21,-1.,1.26069923670246E-19));
#8534=DIRECTION('',(-6.6070447339401E-21,1.,-1.26069923670246E-19));
#8535=DIRECTION('center_axis',(-0.377681861983727,-0.843372107574981,-0.382204002193907));
#8536=DIRECTION('ref_axis',(0.592794689304909,-0.537329962094554,0.599892463836112));
#8537=DIRECTION('center_axis',(-0.0522650609395818,0.0520327192429072,0.997276771780618));
#8538=DIRECTION('ref_axis',(0.998629534754574,0.,0.0523359562429431));
#8539=DIRECTION('center_axis',(2.96465769266612E-15,-1.,0.));
#8540=DIRECTION('ref_axis',(0.,0.,1.));
#8541=DIRECTION('center_axis',(0.995216631131787,0.0976926666577189,1.18580395612125E-14));
#8542=DIRECTION('ref_axis',(0.0975341006448478,-0.993601284365854,0.0569524970297685));
#8543=DIRECTION('center_axis',(-6.60704473394009E-21,-1.,1.26069923670246E-19));
#8544=DIRECTION('ref_axis',(0.688354575693758,0.,0.725374371012284));
#8545=DIRECTION('',(6.60704473394009E-21,1.,-1.26069923670246E-19));
#8546=DIRECTION('',(-6.60704473394009E-21,-1.,1.26069923670246E-19));
#8547=DIRECTION('center_axis',(0.998629534754574,0.,-0.0523359562429438));
#8548=DIRECTION('ref_axis',(-0.0523359562429438,0.,-0.998629534754574));
#8549=DIRECTION('center_axis',(-1.01338750660366E-31,1.26069923670246E-19,
1.));
#8550=DIRECTION('ref_axis',(1.,0.,1.01338750660366E-31));
#8551=DIRECTION('center_axis',(-0.998629534754574,0.,-0.0523359562429438));
#8552=DIRECTION('ref_axis',(-0.0523359562429438,0.,0.998629534754574));
#8553=DIRECTION('axis',(0.,0.,1.));
#8554=DIRECTION('refdir',(1.,0.,0.));
#8555=DIRECTION('center_axis',(0.,0.,-1.));
#8556=DIRECTION('ref_axis',(1.,0.,0.));
#8557=DIRECTION('center_axis',(1.01338750660366E-31,-1.26069923670246E-19,
-1.));
#8558=DIRECTION('ref_axis',(1.,0.,0.));
#8559=DIRECTION('',(0.,0.,-1.));
#8560=DIRECTION('center_axis',(-1.01338750660366E-31,1.26069923670246E-19,
1.));
#8561=DIRECTION('ref_axis',(1.,0.,0.));
#8562=DIRECTION('center_axis',(0.,0.,-1.));
#8563=DIRECTION('ref_axis',(1.,0.,0.));
#8564=DIRECTION('center_axis',(1.01338750660366E-31,-1.26069923670246E-19,
-1.));
#8565=DIRECTION('ref_axis',(1.,0.,0.));
#8566=DIRECTION('',(0.,0.,-1.));
#8567=DIRECTION('center_axis',(-1.01338750660366E-31,1.26069923670246E-19,
1.));
#8568=DIRECTION('ref_axis',(1.,0.,0.));
#8569=DIRECTION('center_axis',(0.,0.,-1.));
#8570=DIRECTION('ref_axis',(1.,0.,0.));
#8571=DIRECTION('center_axis',(1.01338750660366E-31,-1.26069923670246E-19,
-1.));
#8572=DIRECTION('ref_axis',(1.,0.,0.));
#8573=DIRECTION('',(0.,0.,-1.));
#8574=DIRECTION('center_axis',(-1.01338750660366E-31,1.26069923670246E-19,
1.));
#8575=DIRECTION('ref_axis',(1.,0.,0.));
#8576=DIRECTION('center_axis',(0.,0.,-1.));
#8577=DIRECTION('ref_axis',(1.,0.,0.));
#8578=DIRECTION('center_axis',(1.01338750660366E-31,-1.26069923670246E-19,
-1.));
#8579=DIRECTION('ref_axis',(1.,0.,0.));
#8580=DIRECTION('',(0.,0.,-1.));
#8581=DIRECTION('center_axis',(-1.01338750660366E-31,1.26069923670246E-19,
1.));
#8582=DIRECTION('ref_axis',(1.,0.,0.));
#8583=DIRECTION('center_axis',(0.86602540378444,0.499999999999998,0.));
#8584=DIRECTION('ref_axis',(0.499999999999998,-0.86602540378444,0.));
#8585=DIRECTION('',(0.499999999999998,-0.86602540378444,1.09179756551649E-19));
#8586=DIRECTION('',(0.,0.,-1.));
#8587=DIRECTION('',(0.499999999999998,-0.86602540378444,0.));
#8588=DIRECTION('',(0.,0.,-1.));
#8589=DIRECTION('center_axis',(1.60246890531963E-16,1.,0.));
#8590=DIRECTION('ref_axis',(1.,-1.60246890531963E-16,0.));
#8591=DIRECTION('',(1.,-1.60246890531963E-16,1.01358952973624E-31));
#8592=DIRECTION('',(0.,0.,-1.));
#8593=DIRECTION('',(1.,-1.60246890531963E-16,0.));
#8594=DIRECTION('center_axis',(-0.86602540378444,0.499999999999998,0.));
#8595=DIRECTION('ref_axis',(0.499999999999998,0.86602540378444,0.));
#8596=DIRECTION('',(0.499999999999998,0.86602540378444,-1.09179756551548E-19));
#8597=DIRECTION('',(0.,0.,-1.));
#8598=DIRECTION('',(0.499999999999998,0.86602540378444,0.));
#8599=DIRECTION('center_axis',(-0.86602540378444,-0.499999999999998,0.));
#8600=DIRECTION('ref_axis',(-0.499999999999998,0.86602540378444,0.));
#8601=DIRECTION('',(-0.499999999999998,0.86602540378444,-1.09179756551649E-19));
#8602=DIRECTION('',(0.,0.,-1.));
#8603=DIRECTION('',(-0.499999999999998,0.86602540378444,0.));
#8604=DIRECTION('center_axis',(-1.60246890531963E-16,-1.,0.));
#8605=DIRECTION('ref_axis',(-1.,1.60246890531963E-16,0.));
#8606=DIRECTION('',(-1.,1.60246890531963E-16,-1.01358952973624E-31));
#8607=DIRECTION('',(0.,0.,-1.));
#8608=DIRECTION('',(-1.,1.60246890531963E-16,0.));
#8609=DIRECTION('center_axis',(0.86602540378444,-0.499999999999998,0.));
#8610=DIRECTION('ref_axis',(-0.499999999999998,-0.86602540378444,0.));
#8611=DIRECTION('',(-0.499999999999998,-0.86602540378444,1.09179756551548E-19));
#8612=DIRECTION('',(-0.499999999999998,-0.86602540378444,0.));
#8613=DIRECTION('center_axis',(0.,0.,-1.));
#8614=DIRECTION('ref_axis',(-1.,0.,0.));
#8615=DIRECTION('center_axis',(0.,0.,1.));
#8616=DIRECTION('ref_axis',(1.,0.,0.));
#8617=DIRECTION('center_axis',(0.866025403784439,0.5,0.));
#8618=DIRECTION('ref_axis',(0.5,-0.866025403784439,0.));
#8619=DIRECTION('',(0.5,-0.866025403784439,1.09179756551649E-19));
#8620=DIRECTION('',(0.,0.,-1.));
#8621=DIRECTION('',(0.5,-0.866025403784439,0.));
#8622=DIRECTION('',(0.,0.,-1.));
#8623=DIRECTION('center_axis',(1.60246890531964E-16,1.,0.));
#8624=DIRECTION('ref_axis',(1.,-1.60246890531964E-16,0.));
#8625=DIRECTION('',(1.,-1.60246890531964E-16,1.01358952973624E-31));
#8626=DIRECTION('',(0.,0.,-1.));
#8627=DIRECTION('',(1.,-1.60246890531964E-16,0.));
#8628=DIRECTION('center_axis',(-0.866025403784438,0.5,0.));
#8629=DIRECTION('ref_axis',(0.5,0.866025403784438,0.));
#8630=DIRECTION('',(0.5,0.866025403784438,-1.09179756551547E-19));
#8631=DIRECTION('',(0.,0.,-1.));
#8632=DIRECTION('',(0.5,0.866025403784438,0.));
#8633=DIRECTION('center_axis',(-0.866025403784439,-0.499999999999999,0.));
#8634=DIRECTION('ref_axis',(-0.499999999999999,0.866025403784439,0.));
#8635=DIRECTION('',(-0.499999999999999,0.866025403784439,-1.09179756551649E-19));
#8636=DIRECTION('',(0.,0.,-1.));
#8637=DIRECTION('',(-0.499999999999999,0.866025403784439,0.));
#8638=DIRECTION('center_axis',(-1.60246890531964E-16,-1.,0.));
#8639=DIRECTION('ref_axis',(-1.,1.60246890531964E-16,0.));
#8640=DIRECTION('',(-1.,1.60246890531964E-16,-1.01358952973624E-31));
#8641=DIRECTION('',(0.,0.,-1.));
#8642=DIRECTION('',(-1.,1.60246890531964E-16,0.));
#8643=DIRECTION('center_axis',(0.866025403784439,-0.5,0.));
#8644=DIRECTION('ref_axis',(-0.5,-0.866025403784439,0.));
#8645=DIRECTION('',(-0.5,-0.866025403784439,1.09179756551547E-19));
#8646=DIRECTION('',(-0.5,-0.866025403784439,0.));
#8647=DIRECTION('center_axis',(0.,0.,-1.));
#8648=DIRECTION('ref_axis',(-1.,0.,0.));
#8649=DIRECTION('center_axis',(0.,0.,1.));
#8650=DIRECTION('ref_axis',(1.,0.,0.));
#8651=DIRECTION('center_axis',(0.,0.,-1.));
#8652=DIRECTION('ref_axis',(1.,0.,0.));
#8653=DIRECTION('',(0.,0.,-1.));
#8654=DIRECTION('center_axis',(0.,0.,1.));
#8655=DIRECTION('ref_axis',(1.,0.,0.));
#8656=DIRECTION('center_axis',(0.,0.,-1.));
#8657=DIRECTION('ref_axis',(1.,0.,0.));
#8658=DIRECTION('',(0.,0.,-1.));
#8659=DIRECTION('center_axis',(0.,0.,1.));
#8660=DIRECTION('ref_axis',(1.,0.,0.));
#8661=DIRECTION('center_axis',(0.,-1.,0.));
#8662=DIRECTION('ref_axis',(-1.,0.,0.));
#8663=DIRECTION('',(0.0523359562429438,0.,0.998629534754574));
#8664=DIRECTION('',(1.,0.,0.));
#8665=DIRECTION('',(-0.0523359562429438,0.,-0.998629534754574));
#8666=DIRECTION('',(1.,0.,0.));
#8667=DIRECTION('center_axis',(0.,-1.,0.));
#8668=DIRECTION('ref_axis',(-1.,0.,0.));
#8669=DIRECTION('',(0.,0.,-1.));
#8670=DIRECTION('',(1.,0.,0.));
#8671=DIRECTION('',(0.,0.,1.));
#8672=DIRECTION('',(1.,0.,0.));
#8673=DIRECTION('center_axis',(0.,-1.,0.));
#8674=DIRECTION('ref_axis',(-1.,0.,0.));
#8675=DIRECTION('',(0.,0.,-1.));
#8676=DIRECTION('',(1.,0.,0.));
#8677=DIRECTION('',(0.,0.,1.));
#8678=DIRECTION('',(1.,0.,0.));
#8679=DIRECTION('center_axis',(0.,-1.,0.));
#8680=DIRECTION('ref_axis',(-1.,0.,0.));
#8681=DIRECTION('',(0.,0.,-1.));
#8682=DIRECTION('',(1.,0.,0.));
#8683=DIRECTION('',(0.,0.,1.));
#8684=DIRECTION('',(1.,0.,0.));
#8685=DIRECTION('center_axis',(0.,1.,0.));
#8686=DIRECTION('ref_axis',(1.,0.,0.));
#8687=DIRECTION('',(-0.0523359562429438,0.,-0.998629534754574));
#8688=DIRECTION('',(-1.,0.,0.));
#8689=DIRECTION('',(0.0523359562429438,0.,0.998629534754574));
#8690=DIRECTION('',(-1.,0.,0.));
#8691=DIRECTION('center_axis',(0.,1.,0.));
#8692=DIRECTION('ref_axis',(1.,0.,0.));
#8693=DIRECTION('',(0.,0.,1.));
#8694=DIRECTION('',(-1.,0.,0.));
#8695=DIRECTION('',(0.,0.,-1.));
#8696=DIRECTION('',(-1.,0.,0.));
#8697=DIRECTION('center_axis',(0.,1.,0.));
#8698=DIRECTION('ref_axis',(1.,0.,0.));
#8699=DIRECTION('',(0.,0.,1.));
#8700=DIRECTION('',(-1.,0.,0.));
#8701=DIRECTION('',(0.,0.,-1.));
#8702=DIRECTION('',(-1.,0.,0.));
#8703=DIRECTION('center_axis',(0.,0.,1.));
#8704=DIRECTION('ref_axis',(1.,0.,0.));
#8705=DIRECTION('center_axis',(0.,0.,1.));
#8706=DIRECTION('ref_axis',(1.,0.,0.));
#8707=DIRECTION('center_axis',(0.,0.,1.));
#8708=DIRECTION('ref_axis',(1.,0.,0.));
#8709=DIRECTION('center_axis',(0.,0.,1.));
#8710=DIRECTION('ref_axis',(1.,0.,0.));
#8711=DIRECTION('center_axis',(0.,0.,1.));
#8712=DIRECTION('ref_axis',(1.,0.,0.));
#8713=DIRECTION('',(0.,1.,0.));
#8714=DIRECTION('',(0.,-1.,0.));
#8715=DIRECTION('center_axis',(0.,0.,1.));
#8716=DIRECTION('ref_axis',(1.,0.,0.));
#8717=DIRECTION('',(0.,-1.,0.));
#8718=DIRECTION('',(0.,1.,0.));
#8719=DIRECTION('center_axis',(0.,0.,1.));
#8720=DIRECTION('ref_axis',(1.,0.,0.));
#8721=DIRECTION('',(0.,-1.,0.));
#8722=DIRECTION('',(0.,1.,0.));
#8723=DIRECTION('center_axis',(0.,0.,1.));
#8724=DIRECTION('ref_axis',(1.,0.,0.));
#8725=DIRECTION('',(0.,-1.,0.));
#8726=DIRECTION('',(-1.,0.,0.));
#8727=DIRECTION('',(0.,1.,0.));
#8728=DIRECTION('center_axis',(0.,1.,0.));
#8729=DIRECTION('ref_axis',(1.,0.,0.));
#8730=DIRECTION('',(0.,0.,1.));
#8731=DIRECTION('',(-1.,0.,0.));
#8732=DIRECTION('',(0.,0.,-1.));
#8733=DIRECTION('center_axis',(-1.,0.,0.));
#8734=DIRECTION('ref_axis',(0.,-1.,0.));
#8735=DIRECTION('',(0.,-1.,0.));
#8736=DIRECTION('',(0.,-1.,1.26069923670246E-19));
#8737=DIRECTION('center_axis',(1.,0.,0.));
#8738=DIRECTION('ref_axis',(0.,1.,0.));
#8739=DIRECTION('',(0.,1.,0.));
#8740=DIRECTION('',(0.,1.,-1.26069923670246E-19));
#8741=DIRECTION('',(0.,1.,0.));
#8742=DIRECTION('center_axis',(1.,0.,0.));
#8743=DIRECTION('ref_axis',(0.,1.,0.));
#8744=DIRECTION('',(0.,1.,0.));
#8745=DIRECTION('',(0.,1.,-1.26069923670246E-19));
#8746=DIRECTION('',(0.,1.,0.));
#8747=DIRECTION('center_axis',(1.,0.,0.));
#8748=DIRECTION('ref_axis',(0.,1.,0.));
#8749=DIRECTION('',(0.,1.,0.));
#8750=DIRECTION('',(0.,1.,-1.26069923670246E-19));
#8751=DIRECTION('',(0.,1.,0.));
#8752=DIRECTION('center_axis',(0.998629534754574,0.,-0.0523359562429438));
#8753=DIRECTION('ref_axis',(-0.0523359562429438,0.,-0.998629534754574));
#8754=DIRECTION('',(0.,-1.,0.));
#8755=DIRECTION('',(6.6070447339401E-21,-1.,1.26069923670246E-19));
#8756=DIRECTION('',(0.,-1.,0.));
#8757=DIRECTION('center_axis',(0.,0.,1.));
#8758=DIRECTION('ref_axis',(1.,0.,0.));
#8759=DIRECTION('',(0.,-1.,0.));
#8760=DIRECTION('',(0.,-1.,0.));
#8761=DIRECTION('',(0.,-1.,0.));
#8762=DIRECTION('',(0.,1.,0.));
#8763=DIRECTION('',(0.,-1.,0.));
#8764=DIRECTION('',(0.,1.,0.));
#8765=DIRECTION('',(0.,-1.,0.));
#8766=DIRECTION('',(0.,-1.,0.));
#8767=DIRECTION('',(0.,-1.,0.));
#8768=DIRECTION('',(0.,1.,0.));
#8769=DIRECTION('',(0.,1.,0.));
#8770=DIRECTION('center_axis',(0.,0.,1.));
#8771=DIRECTION('ref_axis',(1.,0.,0.));
#8772=DIRECTION('center_axis',(-1.01338750660366E-31,1.26069923670246E-19,
1.));
#8773=DIRECTION('ref_axis',(1.,0.,0.));
#8774=DIRECTION('',(0.,0.,-1.));
#8775=DIRECTION('center_axis',(0.,0.,1.));
#8776=DIRECTION('ref_axis',(1.,0.,0.));
#8777=DIRECTION('center_axis',(-1.01338750660366E-31,1.26069923670246E-19,
1.));
#8778=DIRECTION('ref_axis',(1.,0.,0.));
#8779=DIRECTION('',(0.,0.,-1.));
#8780=DIRECTION('center_axis',(1.,0.,0.));
#8781=DIRECTION('ref_axis',(0.,1.,0.));
#8782=DIRECTION('',(0.,1.,-1.26069923670246E-19));
#8783=DIRECTION('center_axis',(0.995216631131787,0.0976926666577189,1.18580395612125E-14));
#8784=DIRECTION('ref_axis',(0.0975341006448478,-0.993601284365854,0.0569524970297685));
#8785=DIRECTION('center_axis',(-1.01338750660366E-31,1.26069923670246E-19,
1.));
#8786=DIRECTION('ref_axis',(1.,0.,1.01338750660366E-31));
#8787=DIRECTION('center_axis',(-1.01338750660366E-31,1.26069923670246E-19,
1.));
#8788=DIRECTION('ref_axis',(1.,0.,1.01338750660366E-31));
#8789=DIRECTION('',(-6.60704473394009E-21,-1.,1.26069923670246E-19));
#8790=DIRECTION('center_axis',(-1.,0.,0.));
#8791=DIRECTION('ref_axis',(0.,-1.,0.));
#8792=DIRECTION('',(0.,-1.,1.26069923670246E-19));
#8793=DIRECTION('center_axis',(-1.01338750660366E-31,1.26069923670246E-19,
1.));
#8794=DIRECTION('ref_axis',(1.,0.,1.01338750660366E-31));
#8795=DIRECTION('center_axis',(-1.,0.,0.));
#8796=DIRECTION('ref_axis',(0.,-1.,0.));
#8797=DIRECTION('',(0.,-1.,1.26069923670246E-19));
#8798=DIRECTION('center_axis',(-1.01338750660366E-31,1.26069923670246E-19,
1.));
#8799=DIRECTION('ref_axis',(1.,0.,1.01338750660366E-31));
#8800=DIRECTION('center_axis',(-1.,0.,0.));
#8801=DIRECTION('ref_axis',(0.,-1.,0.));
#8802=DIRECTION('',(0.,-1.,1.26069923670246E-19));
#8803=DIRECTION('center_axis',(-0.982258063247475,0.187534256031586,1.45403402392141E-15));
#8804=DIRECTION('ref_axis',(1.48029736616688E-15,0.,1.));
#8805=DIRECTION('center_axis',(-1.01338750660366E-31,1.26069923670246E-19,
1.));
#8806=DIRECTION('ref_axis',(1.,0.,1.01338750660366E-31));
#8807=DIRECTION('',(-6.6070447339401E-21,1.,-1.26069923670246E-19));
#8808=DIRECTION('center_axis',(-0.982258063247479,-0.187534256031562,9.14061384143289E-15));
#8809=DIRECTION('ref_axis',(-0.187187393251729,0.980441281772238,0.0607928680392112));
#8810=DIRECTION('center_axis',(-0.45173408531537,0.373496730537872,-0.810207694632559));
#8811=DIRECTION('ref_axis',(-0.624418441188311,0.516273298501642,0.586142893463867));
#8812=DIRECTION('center_axis',(-2.96465769266614E-15,1.,0.));
#8813=DIRECTION('ref_axis',(0.,0.,1.));
#8814=DIRECTION('center_axis',(0.0522655346583812,-0.0518587053130894,0.997285810873755));
#8815=DIRECTION('ref_axis',(-0.998629534754574,0.,0.0523359562429445));
#8816=DIRECTION('center_axis',(0.377681861983732,-0.843372107574977,0.38220400219391));
#8817=DIRECTION('ref_axis',(0.592794689304902,0.537329962094562,0.599892463836113));
#8818=DIRECTION('center_axis',(0.995216631131786,-0.0976926666577302,0.));
#8819=DIRECTION('ref_axis',(0.,0.,1.));
#8820=DIRECTION('center_axis',(-0.0522650609395843,-0.052032719242908,0.997276771780618));
#8821=DIRECTION('ref_axis',(0.0975341006448596,0.993601284365853,0.0569524970297681));
#8822=DIRECTION('center_axis',(1.55158195278682E-16,1.,-2.96059473233375E-15));
#8823=DIRECTION('ref_axis',(0.998629534754574,0.,0.0523359562429438));
#8824=DIRECTION('center_axis',(-0.45173408531537,-0.373496730537869,-0.810207694632561));
#8825=DIRECTION('ref_axis',(-0.624418441188315,-0.516273298501641,0.586142893463864));
#8826=DIRECTION('center_axis',(0.0522655346583823,0.0518587053130918,0.997285810873755));
#8827=DIRECTION('ref_axis',(-0.187187393251729,-0.980441281772238,0.0607928680392122));
#8828=DIRECTION('center_axis',(-2.71526841737693E-16,-1.,-5.18104078158406E-15));
#8829=DIRECTION('ref_axis',(-0.998629534754574,0.,0.0523359562429439));
#8830=DIRECTION('center_axis',(-6.6070447339401E-21,1.,-1.26069923670246E-19));
#8831=DIRECTION('ref_axis',(-0.688354575693753,0.,0.725374371012289));
#8832=DIRECTION('center_axis',(-0.377681861983722,-0.843372107574983,-0.382204002193908));
#8833=DIRECTION('ref_axis',(0.592794689304909,-0.537329962094554,0.599892463836112));
#8834=DIRECTION('center_axis',(-0.0522650609395818,0.0520327192429072,0.997276771780618));
#8835=DIRECTION('ref_axis',(0.998629534754574,0.,0.0523359562429431));
#8836=DIRECTION('center_axis',(2.96465769266612E-15,-1.,0.));
#8837=DIRECTION('ref_axis',(0.,0.,1.));
#8838=DIRECTION('center_axis',(-6.60704473394009E-21,-1.,1.26069923670246E-19));
#8839=DIRECTION('ref_axis',(0.688354575693758,0.,0.725374371012284));
#8840=DIRECTION('',(6.60704473394009E-21,1.,-1.26069923670246E-19));
#8841=DIRECTION('center_axis',(-0.998629534754574,0.,-0.0523359562429438));
#8842=DIRECTION('ref_axis',(-0.0523359562429438,0.,0.998629534754574));
#8843=DIRECTION('center_axis',(-0.45173408531537,0.373496730537872,-0.81020769463256));
#8844=DIRECTION('ref_axis',(-0.624418441188311,0.516273298501643,0.586142893463866));
#8845=DIRECTION('center_axis',(-2.96465769266614E-15,1.,0.));
#8846=DIRECTION('ref_axis',(0.,0.,1.));
#8847=DIRECTION('center_axis',(-0.982258063247479,-0.187534256031562,9.14061384143289E-15));
#8848=DIRECTION('ref_axis',(-0.187187393251729,0.980441281772238,0.0607928680392111));
#8849=DIRECTION('center_axis',(0.0522655346583812,-0.0518587053130894,0.997285810873755));
#8850=DIRECTION('ref_axis',(-0.998629534754574,0.,0.0523359562429445));
#8851=DIRECTION('center_axis',(0.377681861983731,-0.843372107574978,0.38220400219391));
#8852=DIRECTION('ref_axis',(0.592794689304906,0.537329962094559,0.599892463836111));
#8853=DIRECTION('center_axis',(0.995216631131786,-0.0976926666577302,0.));
#8854=DIRECTION('ref_axis',(0.,0.,1.));
#8855=DIRECTION('center_axis',(1.55158195278682E-16,1.,-2.96059473233375E-15));
#8856=DIRECTION('ref_axis',(0.998629534754574,0.,0.0523359562429438));
#8857=DIRECTION('center_axis',(-0.0522650609395843,-0.052032719242908,0.997276771780618));
#8858=DIRECTION('ref_axis',(0.0975341006448596,0.993601284365853,0.0569524970297681));
#8859=DIRECTION('center_axis',(-0.45173408531537,-0.373496730537868,-0.810207694632561));
#8860=DIRECTION('ref_axis',(-0.624418441188315,-0.516273298501641,0.586142893463864));
#8861=DIRECTION('center_axis',(-0.982258063247475,0.187534256031586,1.45403402392141E-15));
#8862=DIRECTION('ref_axis',(1.48029736616688E-15,0.,1.));
#8863=DIRECTION('center_axis',(-2.71526841737693E-16,-1.,-5.18104078158406E-15));
#8864=DIRECTION('ref_axis',(-0.998629534754574,0.,0.0523359562429439));
#8865=DIRECTION('center_axis',(0.0522655346583823,0.0518587053130918,0.997285810873755));
#8866=DIRECTION('ref_axis',(-0.187187393251729,-0.980441281772238,0.0607928680392122));
#8867=DIRECTION('center_axis',(-6.6070447339401E-21,1.,-1.26069923670246E-19));
#8868=DIRECTION('ref_axis',(-0.688354575693753,0.,0.725374371012289));
#8869=DIRECTION('',(6.6070447339401E-21,-1.,1.26069923670246E-19));
#8870=DIRECTION('',(-6.6070447339401E-21,1.,-1.26069923670246E-19));
#8871=DIRECTION('center_axis',(-0.377681861983727,-0.843372107574981,-0.382204002193907));
#8872=DIRECTION('ref_axis',(0.592794689304909,-0.537329962094554,0.599892463836112));
#8873=DIRECTION('center_axis',(-0.0522650609395818,0.0520327192429072,0.997276771780618));
#8874=DIRECTION('ref_axis',(0.998629534754574,0.,0.0523359562429431));
#8875=DIRECTION('center_axis',(2.96465769266612E-15,-1.,0.));
#8876=DIRECTION('ref_axis',(0.,0.,1.));
#8877=DIRECTION('center_axis',(0.995216631131787,0.0976926666577189,1.18580395612125E-14));
#8878=DIRECTION('ref_axis',(0.0975341006448478,-0.993601284365854,0.0569524970297685));
#8879=DIRECTION('center_axis',(-6.60704473394009E-21,-1.,1.26069923670246E-19));
#8880=DIRECTION('ref_axis',(0.688354575693758,0.,0.725374371012284));
#8881=DIRECTION('',(6.60704473394009E-21,1.,-1.26069923670246E-19));
#8882=DIRECTION('',(-6.60704473394009E-21,-1.,1.26069923670246E-19));
#8883=DIRECTION('center_axis',(0.998629534754574,0.,-0.0523359562429438));
#8884=DIRECTION('ref_axis',(-0.0523359562429438,0.,-0.998629534754574));
#8885=DIRECTION('center_axis',(-1.01338750660366E-31,1.26069923670246E-19,
1.));
#8886=DIRECTION('ref_axis',(1.,0.,1.01338750660366E-31));
#8887=DIRECTION('center_axis',(-0.998629534754574,0.,-0.0523359562429438));
#8888=DIRECTION('ref_axis',(-0.0523359562429438,0.,0.998629534754574));
#8889=DIRECTION('axis',(0.,0.,1.));
#8890=DIRECTION('refdir',(1.,0.,0.));
#8891=DIRECTION('center_axis',(0.,0.,-1.));
#8892=DIRECTION('ref_axis',(1.,0.,0.));
#8893=DIRECTION('center_axis',(-2.77374560774598E-32,-4.07593403759339E-32,
-1.));
#8894=DIRECTION('ref_axis',(1.,0.,0.));
#8895=DIRECTION('',(0.,0.,-1.));
#8896=DIRECTION('center_axis',(-3.68477953769876E-32,1.85992248306542E-19,
1.));
#8897=DIRECTION('ref_axis',(1.,0.,0.));
#8898=DIRECTION('center_axis',(0.,0.,-1.));
#8899=DIRECTION('ref_axis',(1.,0.,0.));
#8900=DIRECTION('center_axis',(-2.77374560774598E-32,-4.07593403759339E-32,
-1.));
#8901=DIRECTION('ref_axis',(1.,0.,0.));
#8902=DIRECTION('',(0.,0.,-1.));
#8903=DIRECTION('center_axis',(-3.68477953769876E-32,1.85992248306542E-19,
1.));
#8904=DIRECTION('ref_axis',(1.,0.,0.));
#8905=DIRECTION('center_axis',(0.,0.,1.));
#8906=DIRECTION('ref_axis',(1.,0.,0.));
#8907=DIRECTION('center_axis',(0.,0.,1.));
#8908=DIRECTION('ref_axis',(1.,0.,0.));
#8909=DIRECTION('center_axis',(0.,0.,-1.));
#8910=DIRECTION('ref_axis',(1.,0.,0.));
#8911=DIRECTION('center_axis',(0.,0.,-1.));
#8912=DIRECTION('ref_axis',(1.,0.,0.));
#8913=DIRECTION('center_axis',(0.,0.,-1.));
#8914=DIRECTION('ref_axis',(1.,0.,0.));
#8915=DIRECTION('',(0.,0.,1.));
#8916=DIRECTION('center_axis',(0.,0.,1.));
#8917=DIRECTION('ref_axis',(1.,0.,0.));
#8918=DIRECTION('center_axis',(0.,0.,1.));
#8919=DIRECTION('ref_axis',(1.,0.,0.));
#8920=DIRECTION('center_axis',(0.,0.,1.));
#8921=DIRECTION('ref_axis',(1.,0.,0.));
#8922=DIRECTION('center_axis',(0.,0.,-1.));
#8923=DIRECTION('ref_axis',(1.,0.,0.));
#8924=DIRECTION('center_axis',(0.,0.,-1.));
#8925=DIRECTION('ref_axis',(1.,0.,0.));
#8926=DIRECTION('center_axis',(0.,0.,-1.));
#8927=DIRECTION('ref_axis',(1.,0.,0.));
#8928=DIRECTION('',(0.,0.,1.));
#8929=DIRECTION('center_axis',(0.,0.,1.));
#8930=DIRECTION('ref_axis',(1.,0.,0.));
#8931=DIRECTION('center_axis',(0.,0.,1.));
#8932=DIRECTION('ref_axis',(1.,0.,0.));
#8933=DIRECTION('center_axis',(0.,0.,1.));
#8934=DIRECTION('ref_axis',(1.,0.,0.));
#8935=DIRECTION('center_axis',(0.,0.,-1.));
#8936=DIRECTION('ref_axis',(1.,0.,0.));
#8937=DIRECTION('center_axis',(0.,0.,-1.));
#8938=DIRECTION('ref_axis',(1.,0.,0.));
#8939=DIRECTION('center_axis',(0.,0.,-1.));
#8940=DIRECTION('ref_axis',(1.,0.,0.));
#8941=DIRECTION('',(0.,0.,1.));
#8942=DIRECTION('center_axis',(0.,0.,1.));
#8943=DIRECTION('ref_axis',(1.,0.,0.));
#8944=DIRECTION('center_axis',(0.,0.,1.));
#8945=DIRECTION('ref_axis',(1.,0.,0.));
#8946=DIRECTION('center_axis',(0.,0.,1.));
#8947=DIRECTION('ref_axis',(1.,0.,0.));
#8948=DIRECTION('center_axis',(0.,0.,-1.));
#8949=DIRECTION('ref_axis',(1.,0.,0.));
#8950=DIRECTION('center_axis',(0.,0.,-1.));
#8951=DIRECTION('ref_axis',(1.,0.,0.));
#8952=DIRECTION('center_axis',(0.,0.,-1.));
#8953=DIRECTION('ref_axis',(1.,0.,0.));
#8954=DIRECTION('',(0.,0.,1.));
#8955=DIRECTION('center_axis',(0.,0.,1.));
#8956=DIRECTION('ref_axis',(1.,0.,0.));
#8957=DIRECTION('center_axis',(0.,0.,-1.));
#8958=DIRECTION('ref_axis',(1.,0.,0.));
#8959=DIRECTION('',(0.,0.,1.));
#8960=DIRECTION('center_axis',(-3.68477953769876E-32,1.85992248306542E-19,
1.));
#8961=DIRECTION('ref_axis',(1.,0.,0.));
#8962=DIRECTION('center_axis',(0.,0.,-1.));
#8963=DIRECTION('ref_axis',(1.,0.,0.));
#8964=DIRECTION('',(0.,0.,1.));
#8965=DIRECTION('center_axis',(-3.68477953769876E-32,1.85992248306542E-19,
1.));
#8966=DIRECTION('ref_axis',(1.,0.,0.));
#8967=DIRECTION('center_axis',(0.,0.,-1.));
#8968=DIRECTION('ref_axis',(1.,0.,0.));
#8969=DIRECTION('',(0.,0.,1.));
#8970=DIRECTION('center_axis',(-3.68477953769876E-32,1.85992248306542E-19,
1.));
#8971=DIRECTION('ref_axis',(1.,0.,0.));
#8972=DIRECTION('center_axis',(0.,0.,-1.));
#8973=DIRECTION('ref_axis',(1.,0.,0.));
#8974=DIRECTION('',(0.,0.,1.));
#8975=DIRECTION('center_axis',(-3.68477953769876E-32,1.85992248306542E-19,
1.));
#8976=DIRECTION('ref_axis',(1.,0.,0.));
#8977=DIRECTION('center_axis',(0.,1.,0.));
#8978=DIRECTION('ref_axis',(0.,0.,1.));
#8979=DIRECTION('center_axis',(0.994535543241646,-0.104398530780106,0.));
#8980=DIRECTION('ref_axis',(0.104226596285684,0.992897637377125,0.0573680949450512));
#8981=DIRECTION('center_axis',(-2.13610651414414E-33,-1.,4.07593403759339E-32));
#8982=DIRECTION('ref_axis',(0.688354575693766,0.,0.725374371012276));
#8983=DIRECTION('center_axis',(0.,1.,0.));
#8984=DIRECTION('ref_axis',(0.,0.,1.));
#8985=DIRECTION('',(2.13610651414414E-33,1.,-4.07593403759339E-32));
#8986=DIRECTION('',(-2.13610651414414E-33,-1.,4.07593403759339E-32));
#8987=DIRECTION('center_axis',(0.994535543241646,0.104398530780106,0.));
#8988=DIRECTION('ref_axis',(0.,0.,1.));
#8989=DIRECTION('center_axis',(0.979252793246429,-0.20264246079997,0.));
#8990=DIRECTION('ref_axis',(0.,0.,1.));
#8991=DIRECTION('center_axis',(0.,-1.,0.));
#8992=DIRECTION('ref_axis',(-2.77555756156289E-15,0.,1.));
#8993=DIRECTION('center_axis',(-2.13610651414429E-33,1.,-4.07593403759339E-32));
#8994=DIRECTION('ref_axis',(-0.688354575693754,0.,0.725374371012288));
#8995=DIRECTION('center_axis',(0.,-1.,0.));
#8996=DIRECTION('ref_axis',(0.,0.,1.));
#8997=DIRECTION('',(2.13610651414429E-33,-1.,4.07593403759339E-32));
#8998=DIRECTION('',(-2.13610651414429E-33,1.,-4.07593403759339E-32));
#8999=DIRECTION('center_axis',(-0.979252793246429,-0.20264246079997,-4.07695874246507E-15));
#9000=DIRECTION('ref_axis',(-4.16333634234434E-15,0.,1.));
#9001=DIRECTION('center_axis',(0.998629534754574,0.,-0.0523359562429439));
#9002=DIRECTION('ref_axis',(-0.0523359562429439,0.,-0.998629534754574));
#9003=DIRECTION('',(0.,1.,0.));
#9004=DIRECTION('center_axis',(2.77374560774598E-32,4.07593403759339E-32,
1.));
#9005=DIRECTION('ref_axis',(1.,0.,-2.77374560774598E-32));
#9006=DIRECTION('center_axis',(-0.998629534754574,0.,-0.0523359562429402));
#9007=DIRECTION('ref_axis',(-0.0523359562429402,0.,0.998629534754574));
#9008=DIRECTION('',(0.,-1.,0.));
#9009=DIRECTION('center_axis',(-3.68477953769876E-32,1.85992248306542E-19,
1.));
#9010=DIRECTION('ref_axis',(1.,0.,3.68477953769876E-32));
#9011=DIRECTION('axis',(0.,0.,1.));
#9012=DIRECTION('refdir',(1.,0.,0.));
#9013=DIRECTION('center_axis',(0.,0.,1.));
#9014=DIRECTION('ref_axis',(1.,0.,0.));
#9015=DIRECTION('',(0.,0.,-1.));
#9016=DIRECTION('center_axis',(0.,0.,-1.));
#9017=DIRECTION('ref_axis',(1.,0.,0.));
#9018=DIRECTION('center_axis',(0.,0.,1.));
#9019=DIRECTION('ref_axis',(1.,0.,0.));
#9020=DIRECTION('',(0.,0.,-1.));
#9021=DIRECTION('center_axis',(0.,0.,1.));
#9022=DIRECTION('ref_axis',(1.,0.,0.));
#9023=DIRECTION('',(0.,0.,-1.));
#9024=DIRECTION('center_axis',(0.,0.,1.));
#9025=DIRECTION('ref_axis',(1.,0.,0.));
#9026=DIRECTION('',(0.,0.,-1.));
#9027=DIRECTION('center_axis',(0.,0.,1.));
#9028=DIRECTION('ref_axis',(1.,0.,0.));
#9029=DIRECTION('',(0.,0.,-1.));
#9030=DIRECTION('center_axis',(0.,0.,1.));
#9031=DIRECTION('ref_axis',(1.,0.,0.));
#9032=DIRECTION('',(0.,0.,-1.));
#9033=DIRECTION('center_axis',(0.,0.,1.));
#9034=DIRECTION('ref_axis',(1.,0.,0.));
#9035=DIRECTION('',(0.,0.,-1.));
#9036=DIRECTION('center_axis',(0.,0.,1.));
#9037=DIRECTION('ref_axis',(1.,0.,0.));
#9038=DIRECTION('',(0.,0.,-1.));
#9039=DIRECTION('center_axis',(0.,0.,1.));
#9040=DIRECTION('ref_axis',(1.,0.,0.));
#9041=DIRECTION('',(0.,0.,-1.));
#9042=DIRECTION('center_axis',(0.,0.,1.));
#9043=DIRECTION('ref_axis',(1.,0.,0.));
#9044=DIRECTION('',(0.,0.,-1.));
#9045=DIRECTION('center_axis',(0.,0.,1.));
#9046=DIRECTION('ref_axis',(1.,0.,0.));
#9047=DIRECTION('',(0.,0.,-1.));
#9048=DIRECTION('center_axis',(0.,0.,1.));
#9049=DIRECTION('ref_axis',(1.,0.,0.));
#9050=DIRECTION('',(0.,0.,-1.));
#9051=DIRECTION('center_axis',(0.,0.,1.));
#9052=DIRECTION('ref_axis',(1.,0.,0.));
#9053=DIRECTION('',(0.,0.,-1.));
#9054=DIRECTION('center_axis',(0.,0.,1.));
#9055=DIRECTION('ref_axis',(1.,0.,0.));
#9056=DIRECTION('',(0.,0.,-1.));
#9057=DIRECTION('center_axis',(0.,0.,1.));
#9058=DIRECTION('ref_axis',(1.,0.,0.));
#9059=DIRECTION('',(0.,0.,-1.));
#9060=DIRECTION('center_axis',(0.,0.,1.));
#9061=DIRECTION('ref_axis',(1.,0.,0.));
#9062=DIRECTION('',(0.,0.,-1.));
#9063=DIRECTION('center_axis',(0.,0.,1.));
#9064=DIRECTION('ref_axis',(1.,0.,0.));
#9065=DIRECTION('',(0.,0.,-1.));
#9066=DIRECTION('center_axis',(0.,0.,1.));
#9067=DIRECTION('ref_axis',(1.,0.,0.));
#9068=DIRECTION('',(0.,0.,-1.));
#9069=DIRECTION('center_axis',(0.,0.,1.));
#9070=DIRECTION('ref_axis',(1.,0.,0.));
#9071=DIRECTION('',(0.,0.,-1.));
#9072=DIRECTION('center_axis',(0.,0.,1.));
#9073=DIRECTION('ref_axis',(1.,0.,0.));
#9074=DIRECTION('',(0.,0.,-1.));
#9075=DIRECTION('center_axis',(0.,0.,1.));
#9076=DIRECTION('ref_axis',(1.,0.,0.));
#9077=DIRECTION('',(0.,0.,-1.));
#9078=DIRECTION('center_axis',(0.,0.,1.));
#9079=DIRECTION('ref_axis',(1.,0.,0.));
#9080=DIRECTION('',(0.,0.,-1.));
#9081=DIRECTION('center_axis',(0.,0.,1.));
#9082=DIRECTION('ref_axis',(1.,0.,0.));
#9083=DIRECTION('',(0.,0.,-1.));
#9084=DIRECTION('center_axis',(0.,0.,1.));
#9085=DIRECTION('ref_axis',(1.,0.,0.));
#9086=DIRECTION('',(0.,0.,-1.));
#9087=DIRECTION('center_axis',(0.,0.,1.));
#9088=DIRECTION('ref_axis',(1.,0.,0.));
#9089=DIRECTION('',(0.,0.,-1.));
#9090=DIRECTION('center_axis',(0.,0.,1.));
#9091=DIRECTION('ref_axis',(1.,0.,0.));
#9092=DIRECTION('',(0.,0.,-1.));
#9093=DIRECTION('center_axis',(0.,0.,1.));
#9094=DIRECTION('ref_axis',(1.,0.,0.));
#9095=DIRECTION('',(0.,0.,-1.));
#9096=DIRECTION('center_axis',(0.,0.,1.));
#9097=DIRECTION('ref_axis',(1.,0.,0.));
#9098=DIRECTION('',(0.,0.,-1.));
#9099=DIRECTION('center_axis',(0.,0.,1.));
#9100=DIRECTION('ref_axis',(1.,0.,0.));
#9101=DIRECTION('',(0.,0.,-1.));
#9102=DIRECTION('center_axis',(0.,0.,1.));
#9103=DIRECTION('ref_axis',(1.,0.,0.));
#9104=DIRECTION('',(0.,0.,-1.));
#9105=DIRECTION('center_axis',(0.,0.,1.));
#9106=DIRECTION('ref_axis',(1.,-2.42503376499884E-13,0.));
#9107=DIRECTION('',(0.,0.,1.));
#9108=DIRECTION('center_axis',(0.,0.,-1.));
#9109=DIRECTION('ref_axis',(1.,-2.42503376499884E-13,0.));
#9110=DIRECTION('center_axis',(0.,0.,1.));
#9111=DIRECTION('ref_axis',(1.,-2.42503376499884E-13,0.));
#9112=DIRECTION('',(0.,0.,1.));
#9113=DIRECTION('center_axis',(0.,0.,1.));
#9114=DIRECTION('ref_axis',(1.,-2.42503376499884E-13,0.));
#9115=DIRECTION('',(0.,0.,1.));
#9116=DIRECTION('center_axis',(0.,0.,1.));
#9117=DIRECTION('ref_axis',(1.,-2.42503376499884E-13,0.));
#9118=DIRECTION('',(0.,0.,1.));
#9119=DIRECTION('center_axis',(0.,0.,1.));
#9120=DIRECTION('ref_axis',(1.,-2.42503376499884E-13,0.));
#9121=DIRECTION('',(0.,0.,1.));
#9122=DIRECTION('center_axis',(0.,0.,1.));
#9123=DIRECTION('ref_axis',(1.,-2.42503376499884E-13,0.));
#9124=DIRECTION('',(0.,0.,1.));
#9125=DIRECTION('center_axis',(0.,0.,1.));
#9126=DIRECTION('ref_axis',(1.,-2.42503376499884E-13,0.));
#9127=DIRECTION('',(0.,0.,1.));
#9128=DIRECTION('center_axis',(0.,0.,1.));
#9129=DIRECTION('ref_axis',(1.,-2.42503376499884E-13,0.));
#9130=DIRECTION('',(0.,0.,1.));
#9131=DIRECTION('center_axis',(0.,0.,1.));
#9132=DIRECTION('ref_axis',(1.,-2.42503376499884E-13,0.));
#9133=DIRECTION('',(0.,0.,1.));
#9134=DIRECTION('center_axis',(0.,0.,1.));
#9135=DIRECTION('ref_axis',(1.,-2.42503376499884E-13,0.));
#9136=DIRECTION('',(0.,0.,1.));
#9137=DIRECTION('center_axis',(0.,0.,1.));
#9138=DIRECTION('ref_axis',(1.,-2.42503376499884E-13,0.));
#9139=DIRECTION('',(0.,0.,1.));
#9140=DIRECTION('center_axis',(0.,0.,1.));
#9141=DIRECTION('ref_axis',(1.,-2.42503376499884E-13,0.));
#9142=DIRECTION('',(0.,0.,1.));
#9143=DIRECTION('center_axis',(0.,0.,1.));
#9144=DIRECTION('ref_axis',(1.,-2.42503376499884E-13,0.));
#9145=DIRECTION('',(0.,0.,1.));
#9146=DIRECTION('center_axis',(0.,0.,1.));
#9147=DIRECTION('ref_axis',(1.,-2.42503376499884E-13,0.));
#9148=DIRECTION('',(0.,0.,1.));
#9149=DIRECTION('center_axis',(0.,0.,1.));
#9150=DIRECTION('ref_axis',(1.,-2.42503376499884E-13,0.));
#9151=DIRECTION('',(0.,0.,1.));
#9152=DIRECTION('center_axis',(0.,0.,1.));
#9153=DIRECTION('ref_axis',(1.,-2.42503376499884E-13,0.));
#9154=DIRECTION('',(0.,0.,1.));
#9155=DIRECTION('center_axis',(0.,0.,1.));
#9156=DIRECTION('ref_axis',(1.,-2.42503376499884E-13,0.));
#9157=DIRECTION('',(0.,0.,1.));
#9158=DIRECTION('center_axis',(0.,0.,1.));
#9159=DIRECTION('ref_axis',(1.,-2.42503376499884E-13,0.));
#9160=DIRECTION('',(0.,0.,1.));
#9161=DIRECTION('center_axis',(0.,0.,1.));
#9162=DIRECTION('ref_axis',(1.,-2.42503376499884E-13,0.));
#9163=DIRECTION('',(0.,0.,1.));
#9164=DIRECTION('center_axis',(0.,0.,1.));
#9165=DIRECTION('ref_axis',(1.,-2.42503376499884E-13,0.));
#9166=DIRECTION('',(0.,0.,1.));
#9167=DIRECTION('center_axis',(0.,0.,1.));
#9168=DIRECTION('ref_axis',(1.,-2.42503376499884E-13,0.));
#9169=DIRECTION('',(0.,0.,1.));
#9170=DIRECTION('center_axis',(0.,0.,1.));
#9171=DIRECTION('ref_axis',(1.,-2.42503376499884E-13,0.));
#9172=DIRECTION('',(0.,0.,1.));
#9173=DIRECTION('center_axis',(0.,0.,1.));
#9174=DIRECTION('ref_axis',(1.,-2.42503376499884E-13,0.));
#9175=DIRECTION('',(0.,0.,1.));
#9176=DIRECTION('center_axis',(0.,0.,1.));
#9177=DIRECTION('ref_axis',(1.,-2.42503376499884E-13,0.));
#9178=DIRECTION('',(0.,0.,1.));
#9179=DIRECTION('center_axis',(0.,0.,1.));
#9180=DIRECTION('ref_axis',(1.,-2.42503376499884E-13,0.));
#9181=DIRECTION('',(0.,0.,1.));
#9182=DIRECTION('center_axis',(0.,0.,1.));
#9183=DIRECTION('ref_axis',(1.,-2.42503376499884E-13,0.));
#9184=DIRECTION('',(0.,0.,1.));
#9185=DIRECTION('center_axis',(0.,0.,1.));
#9186=DIRECTION('ref_axis',(1.,-2.42503376499884E-13,0.));
#9187=DIRECTION('',(0.,0.,1.));
#9188=DIRECTION('center_axis',(0.,0.,1.));
#9189=DIRECTION('ref_axis',(1.,-2.42503376499884E-13,0.));
#9190=DIRECTION('',(0.,0.,1.));
#9191=DIRECTION('center_axis',(0.,0.,1.));
#9192=DIRECTION('ref_axis',(1.,-2.42503376499884E-13,0.));
#9193=DIRECTION('',(0.,0.,1.));
#9194=DIRECTION('center_axis',(0.,0.,1.));
#9195=DIRECTION('ref_axis',(1.,-2.42503376499884E-13,0.));
#9196=DIRECTION('',(0.,0.,1.));
#9197=DIRECTION('center_axis',(0.,0.,-1.));
#9198=DIRECTION('ref_axis',(1.,0.,0.));
#9199=DIRECTION('center_axis',(0.,0.,-1.));
#9200=DIRECTION('ref_axis',(1.,0.,0.));
#9201=DIRECTION('',(0.707106781186547,8.65956056235493E-17,0.707106781186548));
#9202=DIRECTION('center_axis',(0.,0.,1.));
#9203=DIRECTION('ref_axis',(1.,0.,0.));
#9204=DIRECTION('center_axis',(0.,0.,1.));
#9205=DIRECTION('ref_axis',(1.,-2.42503376499884E-13,0.));
#9206=DIRECTION('center_axis',(0.,0.,-1.));
#9207=DIRECTION('ref_axis',(1.,-2.42503376499884E-13,0.));
#9208=DIRECTION('center_axis',(0.,0.,1.));
#9209=DIRECTION('ref_axis',(1.,0.,0.));
#9210=DIRECTION('center_axis',(-1.92296268638356E-16,-1.,0.));
#9211=DIRECTION('ref_axis',(1.,-1.92296268638356E-16,0.));
#9212=DIRECTION('',(1.,-1.92296268638356E-16,0.));
#9213=DIRECTION('',(0.,0.,1.));
#9214=DIRECTION('',(1.,-1.92296268638356E-16,0.));
#9215=DIRECTION('',(0.,0.,1.));
#9216=DIRECTION('center_axis',(-0.866025403784439,-0.5,0.));
#9217=DIRECTION('ref_axis',(0.5,-0.866025403784439,0.));
#9218=DIRECTION('',(0.5,-0.866025403784439,0.));
#9219=DIRECTION('',(0.,0.,1.));
#9220=DIRECTION('',(0.5,-0.866025403784439,0.));
#9221=DIRECTION('center_axis',(-0.866025403784439,0.5,0.));
#9222=DIRECTION('ref_axis',(-0.5,-0.866025403784439,0.));
#9223=DIRECTION('',(-0.5,-0.866025403784439,0.));
#9224=DIRECTION('',(0.,0.,1.));
#9225=DIRECTION('',(-0.5,-0.866025403784438,0.));
#9226=DIRECTION('center_axis',(1.92296268638356E-16,1.,0.));
#9227=DIRECTION('ref_axis',(-1.,1.92296268638356E-16,0.));
#9228=DIRECTION('',(-1.,1.92296268638356E-16,0.));
#9229=DIRECTION('',(0.,0.,1.));
#9230=DIRECTION('',(-1.,1.92296268638356E-16,0.));
#9231=DIRECTION('center_axis',(0.866025403784439,0.5,0.));
#9232=DIRECTION('ref_axis',(-0.5,0.866025403784439,0.));
#9233=DIRECTION('',(-0.5,0.866025403784439,0.));
#9234=DIRECTION('',(0.,0.,1.));
#9235=DIRECTION('',(-0.5,0.866025403784439,0.));
#9236=DIRECTION('center_axis',(0.866025403784439,-0.5,0.));
#9237=DIRECTION('ref_axis',(0.5,0.866025403784439,0.));
#9238=DIRECTION('',(0.5,0.866025403784439,0.));
#9239=DIRECTION('',(0.5,0.866025403784439,0.));
#9240=DIRECTION('center_axis',(0.,0.,1.));
#9241=DIRECTION('ref_axis',(1.,0.,0.));
#9242=DIRECTION('center_axis',(0.,0.,1.));
#9243=DIRECTION('ref_axis',(1.,0.,0.));
#9244=DIRECTION('center_axis',(0.,0.,1.));
#9245=DIRECTION('ref_axis',(1.,0.,0.));
#9246=DIRECTION('center_axis',(0.,0.,1.));
#9247=DIRECTION('ref_axis',(1.,0.,0.));
#9248=DIRECTION('',(0.,0.,-1.));
#9249=DIRECTION('center_axis',(0.,0.,1.));
#9250=DIRECTION('ref_axis',(1.,0.,0.));
#9251=DIRECTION('center_axis',(0.,0.,1.));
#9252=DIRECTION('ref_axis',(1.,0.,0.));
#9253=DIRECTION('center_axis',(0.,0.,1.));
#9254=DIRECTION('ref_axis',(1.,0.,0.));
#9255=DIRECTION('axis',(0.,0.,1.));
#9256=DIRECTION('refdir',(1.,0.,0.));
#9257=DIRECTION('center_axis',(0.,0.,-1.));
#9258=DIRECTION('ref_axis',(1.,0.,0.));
#9259=DIRECTION('',(0.,0.,-1.));
#9260=DIRECTION('center_axis',(0.,0.,-1.));
#9261=DIRECTION('ref_axis',(1.,0.,0.));
#9262=DIRECTION('center_axis',(0.,0.,-1.));
#9263=DIRECTION('ref_axis',(1.,0.,0.));
#9264=DIRECTION('',(0.,0.,-1.));
#9265=DIRECTION('center_axis',(0.,0.,-1.));
#9266=DIRECTION('ref_axis',(1.,0.,0.));
#9267=DIRECTION('center_axis',(0.,0.,-1.));
#9268=DIRECTION('ref_axis',(1.,0.,0.));
#9269=DIRECTION('',(0.,0.,-1.));
#9270=DIRECTION('center_axis',(0.,0.,-1.));
#9271=DIRECTION('ref_axis',(1.,0.,0.));
#9272=DIRECTION('',(0.,0.,-1.));
#9273=DIRECTION('center_axis',(0.,0.,-1.));
#9274=DIRECTION('ref_axis',(0.937385399639056,-0.348293859468591,0.));
#9275=DIRECTION('',(0.,0.,-1.));
#9276=DIRECTION('center_axis',(0.,0.,-1.));
#9277=DIRECTION('ref_axis',(1.,0.,0.));
#9278=DIRECTION('center_axis',(0.,0.,-1.));
#9279=DIRECTION('ref_axis',(0.28361887368566,0.958937085782627,0.));
#9280=DIRECTION('',(1.22464679914735E-16,8.07419868282478E-31,-1.));
#9281=DIRECTION('center_axis',(0.,0.,1.));
#9282=DIRECTION('ref_axis',(1.,6.71554824363804E-15,0.));
#9283=DIRECTION('center_axis',(0.,0.,-1.));
#9284=DIRECTION('ref_axis',(1.,6.71554824363804E-15,0.));
#9285=DIRECTION('',(1.22464679914735E-16,8.07419868282478E-31,-1.));
#9286=DIRECTION('center_axis',(0.,0.,-1.));
#9287=DIRECTION('ref_axis',(1.,6.71554824363804E-15,0.));
#9288=DIRECTION('',(1.22464679914735E-16,8.07419868282478E-31,-1.));
#9289=DIRECTION('center_axis',(0.,0.,-1.));
#9290=DIRECTION('ref_axis',(1.,6.71554824363804E-15,0.));
#9291=DIRECTION('',(1.22464679914735E-16,8.07419868282478E-31,-1.));
#9292=DIRECTION('center_axis',(0.,0.,-1.));
#9293=DIRECTION('ref_axis',(-0.60895050335979,-0.793208222636313,0.));
#9294=DIRECTION('',(1.22464679914735E-16,8.07419868282478E-31,-1.));
#9295=DIRECTION('center_axis',(0.,0.,-1.));
#9296=DIRECTION('ref_axis',(1.,6.71554824363804E-15,0.));
#9297=DIRECTION('center_axis',(0.,0.,-1.));
#9298=DIRECTION('ref_axis',(1.,6.71554824363804E-15,0.));
#9299=DIRECTION('center_axis',(0.,0.,1.));
#9300=DIRECTION('ref_axis',(1.,0.,0.));
#9301=DIRECTION('',(0.5,0.866025403784439,0.));
#9302=DIRECTION('',(-0.5,0.866025403784439,0.));
#9303=DIRECTION('',(-1.,0.,0.));
#9304=DIRECTION('',(-0.5,-0.866025403784439,0.));
#9305=DIRECTION('',(0.5,-0.866025403784439,0.));
#9306=DIRECTION('',(1.,-3.49629579342466E-16,0.));
#9307=DIRECTION('center_axis',(0.,0.,-1.));
#9308=DIRECTION('ref_axis',(1.,0.,0.));
#9309=DIRECTION('center_axis',(-3.49629579342466E-16,-1.,0.));
#9310=DIRECTION('ref_axis',(1.,-3.49629579342466E-16,0.));
#9311=DIRECTION('',(1.,-3.49629579342466E-16,0.));
#9312=DIRECTION('',(0.,0.,1.));
#9313=DIRECTION('',(0.,0.,1.));
#9314=DIRECTION('center_axis',(-0.866025403784439,-0.5,0.));
#9315=DIRECTION('ref_axis',(0.5,-0.866025403784439,0.));
#9316=DIRECTION('',(0.5,-0.866025403784439,0.));
#9317=DIRECTION('',(0.,0.,1.));
#9318=DIRECTION('center_axis',(-0.866025403784439,0.5,0.));
#9319=DIRECTION('ref_axis',(-0.5,-0.866025403784439,0.));
#9320=DIRECTION('',(-0.5,-0.866025403784439,0.));
#9321=DIRECTION('',(0.,0.,1.));
#9322=DIRECTION('center_axis',(0.,1.,0.));
#9323=DIRECTION('ref_axis',(-1.,0.,0.));
#9324=DIRECTION('',(-1.,0.,0.));
#9325=DIRECTION('',(0.,0.,1.));
#9326=DIRECTION('center_axis',(0.866025403784439,0.5,0.));
#9327=DIRECTION('ref_axis',(-0.5,0.866025403784439,0.));
#9328=DIRECTION('',(-0.5,0.866025403784439,0.));
#9329=DIRECTION('',(0.,0.,1.));
#9330=DIRECTION('center_axis',(0.866025403784439,-0.5,0.));
#9331=DIRECTION('ref_axis',(0.5,0.866025403784439,0.));
#9332=DIRECTION('',(0.5,0.866025403784439,0.));
#9333=DIRECTION('center_axis',(0.,0.,1.));
#9334=DIRECTION('ref_axis',(1.,0.,0.));
#9335=DIRECTION('',(0.,0.,1.));
#9336=DIRECTION('',(1.,0.,0.));
#9337=DIRECTION('',(0.,-1.22464679914735E-16,-1.));
#9338=DIRECTION('',(1.,0.,0.));
#9339=DIRECTION('',(0.,0.,1.));
#9340=DIRECTION('',(1.,0.,0.));
#9341=DIRECTION('',(0.,-1.22464679914735E-16,-1.));
#9342=DIRECTION('',(1.,0.,0.));
#9343=DIRECTION('',(0.,0.,1.));
#9344=DIRECTION('',(1.,0.,0.));
#9345=DIRECTION('',(0.,-1.22464679914735E-16,-1.));
#9346=DIRECTION('',(1.,0.,0.));
#9347=DIRECTION('',(0.,-1.22464679914735E-16,-1.));
#9348=DIRECTION('',(1.,0.,0.));
#9349=DIRECTION('',(0.,0.,1.));
#9350=DIRECTION('',(1.,0.,0.));
#9351=DIRECTION('axis',(0.,0.,1.));
#9352=DIRECTION('refdir',(1.,0.,0.));
#9353=DIRECTION('center_axis',(0.,0.,1.));
#9354=DIRECTION('ref_axis',(1.,0.,0.));
#9355=DIRECTION('center_axis',(0.,0.,-1.));
#9356=DIRECTION('ref_axis',(1.,0.,0.));
#9357=DIRECTION('',(0.,0.,-1.));
#9358=DIRECTION('center_axis',(0.,0.,-1.));
#9359=DIRECTION('ref_axis',(1.,0.,0.));
#9360=DIRECTION('center_axis',(0.,0.,1.));
#9361=DIRECTION('ref_axis',(1.,0.,0.));
#9362=DIRECTION('center_axis',(0.,0.,1.));
#9363=DIRECTION('ref_axis',(1.,0.,0.));
#9364=DIRECTION('',(0.,0.,-1.));
#9365=DIRECTION('center_axis',(0.,0.,1.));
#9366=DIRECTION('ref_axis',(1.,0.,0.));
#9367=DIRECTION('center_axis',(0.,0.,1.));
#9368=DIRECTION('ref_axis',(1.,0.,0.));
#9369=DIRECTION('center_axis',(0.,0.,1.));
#9370=DIRECTION('ref_axis',(1.,0.,0.));
#9371=DIRECTION('',(0.,0.,1.));
#9372=DIRECTION('',(1.,0.,0.));
#9373=DIRECTION('',(0.,-1.22464679914735E-16,-1.));
#9374=DIRECTION('',(1.,0.,0.));
#9375=DIRECTION('',(0.,0.,1.));
#9376=DIRECTION('',(1.,0.,0.));
#9377=DIRECTION('',(0.,0.,1.));
#9378=DIRECTION('',(1.,0.,0.));
#9379=DIRECTION('',(0.,0.,1.));
#9380=DIRECTION('',(1.,0.,0.));
#9381=DIRECTION('',(0.,0.,1.));
#9382=DIRECTION('',(1.,0.,0.));
#9383=DIRECTION('',(0.,-1.22464679914735E-16,-1.));
#9384=DIRECTION('',(1.,0.,0.));
#9385=DIRECTION('',(0.,0.,1.));
#9386=DIRECTION('',(1.,0.,0.));
#9387=CARTESIAN_POINT('',(0.,0.,0.));
#9388=CARTESIAN_POINT('',(0.,0.,0.));
#9389=CARTESIAN_POINT('Origin',(6.,-2.5,0.3));
#9390=CARTESIAN_POINT('',(5.83,-2.5,0.6));
#9391=CARTESIAN_POINT('Origin',(6.,-2.5,0.6));
#9392=CARTESIAN_POINT('',(5.83,-2.5,0.));
#9393=CARTESIAN_POINT('',(5.83,-2.5,0.3));
#9394=CARTESIAN_POINT('Origin',(6.,-2.5,0.));
#9395=CARTESIAN_POINT('Origin',(14.,-2.5,0.3));
#9396=CARTESIAN_POINT('',(13.83,-2.5,0.6));
#9397=CARTESIAN_POINT('Origin',(14.,-2.5,0.6));
#9398=CARTESIAN_POINT('',(13.83,-2.5,0.));
#9399=CARTESIAN_POINT('',(13.83,-2.5,0.3));
#9400=CARTESIAN_POINT('Origin',(14.,-2.5,0.));
#9401=CARTESIAN_POINT('Origin',(0.,0.,0.3));
#9402=CARTESIAN_POINT('',(-0.41,5.02105187650415E-17,0.6));
#9403=CARTESIAN_POINT('Origin',(0.,0.,0.6));
#9404=CARTESIAN_POINT('',(-0.41,5.02105187650415E-17,0.));
#9405=CARTESIAN_POINT('',(-0.41,5.02105187650415E-17,0.3));
#9406=CARTESIAN_POINT('Origin',(0.,0.,0.));
#9407=CARTESIAN_POINT('Origin',(-2.2,-0.025,0.975));
#9408=CARTESIAN_POINT('',(-2.2,0.2,1.1));
#9409=CARTESIAN_POINT('',(-2.2,-0.2,1.1));
#9410=CARTESIAN_POINT('',(-2.2,0.2875,1.1));
#9411=CARTESIAN_POINT('',(-2.2,-0.2,0.8));
#9412=CARTESIAN_POINT('',(-2.2,-0.2,0.8));
#9413=CARTESIAN_POINT('',(-2.2,-0.2,0.8));
#9414=CARTESIAN_POINT('Origin',(-6.8,-0.2,0.8));
#9415=CARTESIAN_POINT('',(-6.8,-0.2,0.8));
#9416=CARTESIAN_POINT('',(-6.8,0.199999999999998,1.1));
#9417=CARTESIAN_POINT('',(-6.8,-0.2,0.8));
#9418=CARTESIAN_POINT('',(-2.2,-0.2,0.8));
#9419=CARTESIAN_POINT('',(-4.3,0.2,1.1));
#9420=CARTESIAN_POINT('Origin',(-6.8,-0.025,0.975));
#9421=CARTESIAN_POINT('',(-6.8,-0.2,1.1));
#9422=CARTESIAN_POINT('',(-6.8,0.2875,1.1));
#9423=CARTESIAN_POINT('',(-6.8,-0.2,0.8));
#9424=CARTESIAN_POINT('Origin',(-1.8,0.6,1.1));
#9425=CARTESIAN_POINT('',(-2.,0.0666666666666668,1.1));
#9426=CARTESIAN_POINT('',(-1.6,0.6,1.1));
#9427=CARTESIAN_POINT('',(-2.,0.,1.1));
#9428=CARTESIAN_POINT('',(-2.,0.,1.1));
#9429=CARTESIAN_POINT('',(-1.6,0.,1.1));
#9430=CARTESIAN_POINT('',(-1.6,0.,1.1));
#9431=CARTESIAN_POINT('',(-1.6,1.2,1.1));
#9432=CARTESIAN_POINT('',(-1.6,1.2,1.1));
#9433=CARTESIAN_POINT('',(-2.4,1.2,1.1));
#9434=CARTESIAN_POINT('',(-2.,1.2,1.1));
#9435=CARTESIAN_POINT('Origin',(-0.70745614035088,-16.4271929824561,1.1));
#9436=CARTESIAN_POINT('Origin',(-2.2,-0.2,0.8));
#9437=CARTESIAN_POINT('',(-2.,0.0666666666666669,0.8));
#9438=CARTESIAN_POINT('',(-2.,0.0666666666666667,0.4));
#9439=CARTESIAN_POINT('',(-1.6,0.6,0.8));
#9440=CARTESIAN_POINT('Origin',(-6.8,1.38777878078145E-17,0.8));
#9441=CARTESIAN_POINT('',(-6.8,0.199999999999998,0.8));
#9442=CARTESIAN_POINT('Origin',(-6.8,1.38777878078145E-17,0.8));
#9443=CARTESIAN_POINT('Origin',(-6.8,1.38777878078145E-17,1.1));
#9444=CARTESIAN_POINT('',(-6.8,0.199999999999998,0.8));
#9445=CARTESIAN_POINT('Origin',(-0.70745614035088,-16.4271929824561,0.8));
#9446=CARTESIAN_POINT('',(-2.4,1.2,0.8));
#9447=CARTESIAN_POINT('Origin',(-0.70745614035088,-16.4271929824561,0.8));
#9448=CARTESIAN_POINT('',(-2.4,1.2,0.8));
#9449=CARTESIAN_POINT('Origin',(-4.3,0.5,0.8));
#9450=CARTESIAN_POINT('',(-2.,1.2,0.8));
#9451=CARTESIAN_POINT('',(-2.,0.85,0.8));
#9452=CARTESIAN_POINT('',(-2.4,1.2,0.8));
#9453=CARTESIAN_POINT('Origin',(-2.,1.2,0.));
#9454=CARTESIAN_POINT('',(-2.,1.2,0.));
#9455=CARTESIAN_POINT('',(-2.,1.2,0.));
#9456=CARTESIAN_POINT('',(-2.,0.,0.));
#9457=CARTESIAN_POINT('',(-2.,0.,0.));
#9458=CARTESIAN_POINT('',(-2.,0.,0.));
#9459=CARTESIAN_POINT('Origin',(-1.2,1.2,0.));
#9460=CARTESIAN_POINT('',(-1.6,1.2,0.6));
#9461=CARTESIAN_POINT('',(-1.6,1.2,0.));
#9462=CARTESIAN_POINT('',(-1.2,1.2,0.6));
#9463=CARTESIAN_POINT('',(-2.,1.2,0.6));
#9464=CARTESIAN_POINT('',(-1.2,1.2,0.));
#9465=CARTESIAN_POINT('',(-1.2,1.2,0.));
#9466=CARTESIAN_POINT('',(-2.,1.2,0.));
#9467=CARTESIAN_POINT('Origin',(-1.6,0.,0.));
#9468=CARTESIAN_POINT('',(-1.6,0.,0.6));
#9469=CARTESIAN_POINT('',(-1.6,0.,0.));
#9470=CARTESIAN_POINT('',(-1.6,0.,0.6));
#9471=CARTESIAN_POINT('Origin',(-1.8,0.6,1.1));
#9472=CARTESIAN_POINT('Origin',(-2.,0.,0.));
#9473=CARTESIAN_POINT('',(-1.4,0.,0.));
#9474=CARTESIAN_POINT('',(-1.2,0.,0.));
#9475=CARTESIAN_POINT('',(-1.4,0.,0.6));
#9476=CARTESIAN_POINT('',(-1.4,0.,0.));
#9477=CARTESIAN_POINT('',(-1.2,0.,0.6));
#9478=CARTESIAN_POINT('Origin',(0.,0.,0.));
#9479=CARTESIAN_POINT('',(-1.2,0.721110255092798,0.));
#9480=CARTESIAN_POINT('',(-1.2,1.2,0.));
#9481=CARTESIAN_POINT('',(0.993295878967653,0.986591757935306,0.));
#9482=CARTESIAN_POINT('Origin',(0.,0.,0.));
#9483=CARTESIAN_POINT('',(1.,1.,0.));
#9484=CARTESIAN_POINT('',(1.,1.,0.));
#9485=CARTESIAN_POINT('',(2.26270761578574,-0.307804316349519,0.));
#9486=CARTESIAN_POINT('',(3.8,-1.9,0.));
#9487=CARTESIAN_POINT('',(3.79686161498349,-1.89674952980433,0.));
#9488=CARTESIAN_POINT('Origin',(2.1,-2.,0.));
#9489=CARTESIAN_POINT('',(3.8,-1.9,0.));
#9490=CARTESIAN_POINT('',(3.8,-1.9,0.));
#9491=CARTESIAN_POINT('',(15.2,-1.9,0.));
#9492=CARTESIAN_POINT('',(15.2,-1.9,0.));
#9493=CARTESIAN_POINT('',(15.2,-3.1,0.));
#9494=CARTESIAN_POINT('',(15.2,-3.1,0.));
#9495=CARTESIAN_POINT('',(3.8,-3.1,0.));
#9496=CARTESIAN_POINT('',(3.8,-3.1,0.));
#9497=CARTESIAN_POINT('',(3.51486278039743,-2.94242416811437,0.));
#9498=CARTESIAN_POINT('',(0.,-1.,0.));
#9499=CARTESIAN_POINT('',(0.549222100239177,-1.30351747644797,0.));
#9500=CARTESIAN_POINT('Origin',(2.1,-2.,0.));
#9501=CARTESIAN_POINT('',(0.533017816115691,-1.29456247732709,0.));
#9502=CARTESIAN_POINT('',(0.,-1.,0.));
#9503=CARTESIAN_POINT('Origin',(0.,0.,0.));
#9504=CARTESIAN_POINT('',(0.9,-2.,0.));
#9505=CARTESIAN_POINT('Origin',(2.1,-2.,0.));
#9506=CARTESIAN_POINT('Origin',(-1.2,0.,0.));
#9507=CARTESIAN_POINT('',(-1.2,0.721110255092798,0.6));
#9508=CARTESIAN_POINT('',(-1.2,0.721110255092798,0.));
#9509=CARTESIAN_POINT('',(-1.2,1.2,0.6));
#9510=CARTESIAN_POINT('Origin',(0.,0.,0.));
#9511=CARTESIAN_POINT('',(0.533017816115691,-1.29456247732709,0.6));
#9512=CARTESIAN_POINT('',(0.533017816115691,-1.29456247732709,0.));
#9513=CARTESIAN_POINT('Origin',(0.,0.,0.6));
#9514=CARTESIAN_POINT('Origin',(0.,0.,0.));
#9515=CARTESIAN_POINT('',(0.993295878967653,0.986591757935306,0.6));
#9516=CARTESIAN_POINT('Origin',(0.,0.,0.6));
#9517=CARTESIAN_POINT('',(0.993295878967653,0.986591757935306,0.));
#9518=CARTESIAN_POINT('Origin',(0.,0.,0.6));
#9519=CARTESIAN_POINT('',(0.549222100239177,-1.30351747644797,0.6));
#9520=CARTESIAN_POINT('',(0.,-1.,0.6));
#9521=CARTESIAN_POINT('',(3.51486278039743,-2.94242416811437,0.6));
#9522=CARTESIAN_POINT('Origin',(2.1,-2.,0.6));
#9523=CARTESIAN_POINT('',(3.8,-3.1,0.6));
#9524=CARTESIAN_POINT('',(0.,-1.,0.6));
#9525=CARTESIAN_POINT('',(15.2,-3.1,0.6));
#9526=CARTESIAN_POINT('',(3.8,-3.1,0.6));
#9527=CARTESIAN_POINT('',(15.2,-1.9,0.6));
#9528=CARTESIAN_POINT('',(15.2,-3.1,0.6));
#9529=CARTESIAN_POINT('',(3.8,-1.9,0.6));
#9530=CARTESIAN_POINT('',(15.2,-1.9,0.6));
#9531=CARTESIAN_POINT('',(3.79686161498349,-1.89674952980433,0.6));
#9532=CARTESIAN_POINT('',(3.8,-1.9,0.6));
#9533=CARTESIAN_POINT('',(2.26270761578574,-0.307804316349519,0.6));
#9534=CARTESIAN_POINT('Origin',(2.1,-2.,0.6));
#9535=CARTESIAN_POINT('',(1.,1.,0.6));
#9536=CARTESIAN_POINT('',(3.8,-1.9,0.6));
#9537=CARTESIAN_POINT('',(1.,1.,0.6));
#9538=CARTESIAN_POINT('',(3.3,-2.,0.6));
#9539=CARTESIAN_POINT('Origin',(2.1,-2.,0.6));
#9540=CARTESIAN_POINT('Origin',(2.1,-2.,0.1));
#9541=CARTESIAN_POINT('',(1.,-2.,0.1));
#9542=CARTESIAN_POINT('Origin',(0.9,-2.,0.1));
#9543=CARTESIAN_POINT('Origin',(2.1,-2.,0.1));
#9544=CARTESIAN_POINT('Origin',(2.1,-2.,0.3));
#9545=CARTESIAN_POINT('',(3.2,-2.,0.5));
#9546=CARTESIAN_POINT('',(1.,-2.,0.5));
#9547=CARTESIAN_POINT('Origin',(2.1,-2.,0.5));
#9548=CARTESIAN_POINT('Origin',(2.1,-2.,0.5));
#9549=CARTESIAN_POINT('',(1.,-2.,0.3));
#9550=CARTESIAN_POINT('Origin',(2.1,-2.,0.5));
#9551=CARTESIAN_POINT('Origin',(3.3,-2.,0.5));
#9552=CARTESIAN_POINT('Origin',(2.1,-2.,0.));
#9553=CARTESIAN_POINT('',(2.26270761578574,-0.307804316349519,0.));
#9554=CARTESIAN_POINT('',(3.79686161498349,-1.89674952980433,0.));
#9555=CARTESIAN_POINT('Origin',(2.1,-2.,0.));
#9556=CARTESIAN_POINT('',(0.549222100239177,-1.30351747644797,0.));
#9557=CARTESIAN_POINT('',(3.51486278039743,-2.94242416811437,0.));
#9558=CARTESIAN_POINT('Origin',(0.,-1.,0.));
#9559=CARTESIAN_POINT('',(3.8,-3.1,0.));
#9560=CARTESIAN_POINT('Origin',(3.8,-1.9,0.));
#9561=CARTESIAN_POINT('',(3.8,-1.9,0.));
#9562=CARTESIAN_POINT('Origin',(0.,-1.,0.));
#9563=CARTESIAN_POINT('Origin',(1.,1.,0.));
#9564=CARTESIAN_POINT('',(1.,1.,0.));
#9565=CARTESIAN_POINT('Origin',(3.8,-1.9,0.));
#9566=CARTESIAN_POINT('Origin',(15.2,-1.9,0.));
#9567=CARTESIAN_POINT('',(15.2,-1.9,0.));
#9568=CARTESIAN_POINT('Origin',(15.2,-3.1,0.));
#9569=CARTESIAN_POINT('',(15.2,-3.1,0.));
#9570=CARTESIAN_POINT('Origin',(3.8,-3.1,0.));
#9571=CARTESIAN_POINT('',(0.,0.,0.));
#9572=CARTESIAN_POINT('Origin',(6.,-2.5,0.3));
#9573=CARTESIAN_POINT('',(5.83,-2.5,0.6));
#9574=CARTESIAN_POINT('Origin',(6.,-2.5,0.6));
#9575=CARTESIAN_POINT('',(5.83,-2.5,0.));
#9576=CARTESIAN_POINT('',(5.83,-2.5,0.3));
#9577=CARTESIAN_POINT('Origin',(6.,-2.5,0.));
#9578=CARTESIAN_POINT('Origin',(14.,-2.5,0.3));
#9579=CARTESIAN_POINT('',(13.83,-2.5,0.6));
#9580=CARTESIAN_POINT('Origin',(14.,-2.5,0.6));
#9581=CARTESIAN_POINT('',(13.83,-2.5,0.));
#9582=CARTESIAN_POINT('',(13.83,-2.5,0.3));
#9583=CARTESIAN_POINT('Origin',(14.,-2.5,0.));
#9584=CARTESIAN_POINT('Origin',(0.,0.,0.3));
#9585=CARTESIAN_POINT('',(-0.41,5.02105187650415E-17,0.6));
#9586=CARTESIAN_POINT('Origin',(0.,0.,0.6));
#9587=CARTESIAN_POINT('',(-0.41,5.02105187650415E-17,0.));
#9588=CARTESIAN_POINT('',(-0.41,5.02105187650415E-17,0.3));
#9589=CARTESIAN_POINT('Origin',(0.,0.,0.));
#9590=CARTESIAN_POINT('Origin',(-2.2,-0.025,-0.625));
#9591=CARTESIAN_POINT('',(-2.2,0.2,-0.5));
#9592=CARTESIAN_POINT('',(-2.2,-0.2,-0.5));
#9593=CARTESIAN_POINT('',(-2.2,0.2375,-0.5));
#9594=CARTESIAN_POINT('',(-2.2,-0.2,-0.8));
#9595=CARTESIAN_POINT('',(-2.2,-0.2,-0.8));
#9596=CARTESIAN_POINT('',(-2.2,-0.2,-0.8));
#9597=CARTESIAN_POINT('Origin',(-6.8,-0.2,-0.8));
#9598=CARTESIAN_POINT('',(-6.8,-0.2,-0.8));
#9599=CARTESIAN_POINT('',(-6.8,0.199999999999998,-0.5));
#9600=CARTESIAN_POINT('',(-6.8,-0.2,-0.8));
#9601=CARTESIAN_POINT('',(-2.2,-0.2,-0.8));
#9602=CARTESIAN_POINT('',(-5.55,0.2,-0.5));
#9603=CARTESIAN_POINT('Origin',(-6.8,-0.025,-0.625));
#9604=CARTESIAN_POINT('',(-6.8,-0.2,-0.5));
#9605=CARTESIAN_POINT('',(-6.8,0.2375,-0.5));
#9606=CARTESIAN_POINT('',(-6.8,-0.2,-0.8));
#9607=CARTESIAN_POINT('Origin',(-4.3,0.5,-0.5));
#9608=CARTESIAN_POINT('',(-2.,0.0666666666666669,-0.5));
#9609=CARTESIAN_POINT('',(-1.6,0.6,-0.5));
#9610=CARTESIAN_POINT('',(-2.,1.2,-0.5));
#9611=CARTESIAN_POINT('',(-2.,0.85,-0.5));
#9612=CARTESIAN_POINT('',(-2.4,1.2,-0.5));
#9613=CARTESIAN_POINT('',(-2.4,1.2,-0.5));
#9614=CARTESIAN_POINT('Origin',(-0.70745614035088,-16.4271929824561,-0.5));
#9615=CARTESIAN_POINT('Origin',(-4.3,0.5,-0.5));
#9616=CARTESIAN_POINT('Origin',(-6.8,1.38777878078145E-17,-0.5));
#9617=CARTESIAN_POINT('Origin',(-2.2,-0.2,-0.8));
#9618=CARTESIAN_POINT('',(-2.,0.0666666666666668,-0.8));
#9619=CARTESIAN_POINT('',(-2.,0.0666666666666667,-0.4));
#9620=CARTESIAN_POINT('',(-1.6,0.6,-0.8));
#9621=CARTESIAN_POINT('Origin',(-6.8,1.38777878078145E-17,-0.8));
#9622=CARTESIAN_POINT('',(-6.8,0.199999999999998,-0.8));
#9623=CARTESIAN_POINT('Origin',(-6.8,1.38777878078145E-17,-0.8));
#9624=CARTESIAN_POINT('',(-6.8,0.199999999999998,-0.8));
#9625=CARTESIAN_POINT('Origin',(-0.70745614035088,-16.4271929824561,-0.8));
#9626=CARTESIAN_POINT('',(-2.4,1.2,-0.8));
#9627=CARTESIAN_POINT('Origin',(-0.70745614035088,-16.4271929824561,-0.8));
#9628=CARTESIAN_POINT('',(-2.4,1.2,-0.8));
#9629=CARTESIAN_POINT('Origin',(-1.8,0.6,-0.8));
#9630=CARTESIAN_POINT('',(-1.6,1.2,-0.8));
#9631=CARTESIAN_POINT('',(-1.6,0.,-0.8));
#9632=CARTESIAN_POINT('',(-1.6,1.2,-0.8));
#9633=CARTESIAN_POINT('',(-2.,0.,-0.8));
#9634=CARTESIAN_POINT('',(-1.6,0.,-0.8));
#9635=CARTESIAN_POINT('',(-2.,0.,-0.8));
#9636=CARTESIAN_POINT('',(-2.,1.2,-0.8));
#9637=CARTESIAN_POINT('Origin',(-1.6,0.,-0.8));
#9638=CARTESIAN_POINT('',(-1.6,1.2,0.));
#9639=CARTESIAN_POINT('',(-1.6,1.2,-0.8));
#9640=CARTESIAN_POINT('',(-1.6,0.,0.));
#9641=CARTESIAN_POINT('',(-1.6,0.,0.));
#9642=CARTESIAN_POINT('',(-1.6,0.,-0.8));
#9643=CARTESIAN_POINT('Origin',(-2.,0.,0.));
#9644=CARTESIAN_POINT('',(-1.4,0.,0.));
#9645=CARTESIAN_POINT('',(-1.2,0.,0.));
#9646=CARTESIAN_POINT('',(-1.4,0.,0.6));
#9647=CARTESIAN_POINT('',(-1.4,0.,0.));
#9648=CARTESIAN_POINT('',(-2.,0.,0.6));
#9649=CARTESIAN_POINT('',(-1.2,0.,0.6));
#9650=CARTESIAN_POINT('',(-2.,0.,0.));
#9651=CARTESIAN_POINT('Origin',(0.,0.,0.));
#9652=CARTESIAN_POINT('',(-1.2,1.2,0.));
#9653=CARTESIAN_POINT('',(-2.,1.2,0.));
#9654=CARTESIAN_POINT('',(-1.2,0.721110255092798,0.));
#9655=CARTESIAN_POINT('',(-1.2,1.2,0.));
#9656=CARTESIAN_POINT('',(0.993295878967653,0.986591757935306,0.));
#9657=CARTESIAN_POINT('Origin',(0.,0.,0.));
#9658=CARTESIAN_POINT('',(1.,1.,0.));
#9659=CARTESIAN_POINT('',(1.,1.,0.));
#9660=CARTESIAN_POINT('',(2.26270761578574,-0.307804316349519,0.));
#9661=CARTESIAN_POINT('',(3.8,-1.9,0.));
#9662=CARTESIAN_POINT('',(3.79686161498349,-1.89674952980433,0.));
#9663=CARTESIAN_POINT('Origin',(2.1,-2.,0.));
#9664=CARTESIAN_POINT('',(3.8,-1.9,0.));
#9665=CARTESIAN_POINT('',(3.8,-1.9,0.));
#9666=CARTESIAN_POINT('',(15.2,-1.9,0.));
#9667=CARTESIAN_POINT('',(15.2,-1.9,0.));
#9668=CARTESIAN_POINT('',(15.2,-3.1,0.));
#9669=CARTESIAN_POINT('',(15.2,-3.1,0.));
#9670=CARTESIAN_POINT('',(3.8,-3.1,0.));
#9671=CARTESIAN_POINT('',(3.8,-3.1,0.));
#9672=CARTESIAN_POINT('',(3.51486278039743,-2.94242416811437,0.));
#9673=CARTESIAN_POINT('',(0.,-1.,0.));
#9674=CARTESIAN_POINT('',(0.549222100239177,-1.30351747644797,0.));
#9675=CARTESIAN_POINT('Origin',(2.1,-2.,0.));
#9676=CARTESIAN_POINT('',(0.533017816115691,-1.29456247732709,0.));
#9677=CARTESIAN_POINT('',(0.,-1.,0.));
#9678=CARTESIAN_POINT('Origin',(0.,0.,0.));
#9679=CARTESIAN_POINT('',(0.9,-2.,0.));
#9680=CARTESIAN_POINT('Origin',(2.1,-2.,0.));
#9681=CARTESIAN_POINT('Origin',(-1.2,1.2,0.));
#9682=CARTESIAN_POINT('',(-2.,1.2,0.6));
#9683=CARTESIAN_POINT('',(-2.,1.2,0.));
#9684=CARTESIAN_POINT('',(-1.2,1.2,0.6));
#9685=CARTESIAN_POINT('',(-2.,1.2,0.6));
#9686=CARTESIAN_POINT('',(-1.2,1.2,0.));
#9687=CARTESIAN_POINT('Origin',(-2.,1.2,0.));
#9688=CARTESIAN_POINT('',(-2.,0.,0.6));
#9689=CARTESIAN_POINT('Origin',(-1.2,0.,0.));
#9690=CARTESIAN_POINT('',(-1.2,0.721110255092798,0.6));
#9691=CARTESIAN_POINT('',(-1.2,0.721110255092798,0.));
#9692=CARTESIAN_POINT('',(-1.2,1.2,0.6));
#9693=CARTESIAN_POINT('Origin',(0.,0.,0.));
#9694=CARTESIAN_POINT('',(0.533017816115691,-1.29456247732709,0.6));
#9695=CARTESIAN_POINT('',(0.533017816115691,-1.29456247732709,0.));
#9696=CARTESIAN_POINT('Origin',(0.,0.,0.6));
#9697=CARTESIAN_POINT('Origin',(0.,0.,0.));
#9698=CARTESIAN_POINT('',(0.993295878967653,0.986591757935306,0.6));
#9699=CARTESIAN_POINT('Origin',(0.,0.,0.6));
#9700=CARTESIAN_POINT('',(0.993295878967653,0.986591757935306,0.));
#9701=CARTESIAN_POINT('Origin',(0.,0.,0.6));
#9702=CARTESIAN_POINT('',(0.549222100239177,-1.30351747644797,0.6));
#9703=CARTESIAN_POINT('',(0.,-1.,0.6));
#9704=CARTESIAN_POINT('',(3.51486278039743,-2.94242416811437,0.6));
#9705=CARTESIAN_POINT('Origin',(2.1,-2.,0.6));
#9706=CARTESIAN_POINT('',(3.8,-3.1,0.6));
#9707=CARTESIAN_POINT('',(0.,-1.,0.6));
#9708=CARTESIAN_POINT('',(15.2,-3.1,0.6));
#9709=CARTESIAN_POINT('',(3.8,-3.1,0.6));
#9710=CARTESIAN_POINT('',(15.2,-1.9,0.6));
#9711=CARTESIAN_POINT('',(15.2,-3.1,0.6));
#9712=CARTESIAN_POINT('',(3.8,-1.9,0.6));
#9713=CARTESIAN_POINT('',(15.2,-1.9,0.6));
#9714=CARTESIAN_POINT('',(3.79686161498349,-1.89674952980433,0.6));
#9715=CARTESIAN_POINT('',(3.8,-1.9,0.6));
#9716=CARTESIAN_POINT('',(2.26270761578574,-0.307804316349519,0.6));
#9717=CARTESIAN_POINT('Origin',(2.1,-2.,0.6));
#9718=CARTESIAN_POINT('',(1.,1.,0.6));
#9719=CARTESIAN_POINT('',(3.8,-1.9,0.6));
#9720=CARTESIAN_POINT('',(1.,1.,0.6));
#9721=CARTESIAN_POINT('',(3.3,-2.,0.6));
#9722=CARTESIAN_POINT('Origin',(2.1,-2.,0.6));
#9723=CARTESIAN_POINT('Origin',(2.1,-2.,0.1));
#9724=CARTESIAN_POINT('',(1.,-2.,0.1));
#9725=CARTESIAN_POINT('Origin',(0.9,-2.,0.1));
#9726=CARTESIAN_POINT('Origin',(2.1,-2.,0.1));
#9727=CARTESIAN_POINT('Origin',(2.1,-2.,0.3));
#9728=CARTESIAN_POINT('',(3.2,-2.,0.5));
#9729=CARTESIAN_POINT('',(1.,-2.,0.5));
#9730=CARTESIAN_POINT('Origin',(2.1,-2.,0.5));
#9731=CARTESIAN_POINT('Origin',(2.1,-2.,0.5));
#9732=CARTESIAN_POINT('',(1.,-2.,0.3));
#9733=CARTESIAN_POINT('Origin',(2.1,-2.,0.5));
#9734=CARTESIAN_POINT('Origin',(3.3,-2.,0.5));
#9735=CARTESIAN_POINT('Origin',(2.1,-2.,0.));
#9736=CARTESIAN_POINT('',(2.26270761578574,-0.307804316349519,0.));
#9737=CARTESIAN_POINT('',(3.79686161498349,-1.89674952980433,0.));
#9738=CARTESIAN_POINT('Origin',(2.1,-2.,0.));
#9739=CARTESIAN_POINT('',(0.549222100239177,-1.30351747644797,0.));
#9740=CARTESIAN_POINT('',(3.51486278039743,-2.94242416811437,0.));
#9741=CARTESIAN_POINT('Origin',(0.,-1.,0.));
#9742=CARTESIAN_POINT('',(3.8,-3.1,0.));
#9743=CARTESIAN_POINT('Origin',(3.8,-1.9,0.));
#9744=CARTESIAN_POINT('',(3.8,-1.9,0.));
#9745=CARTESIAN_POINT('Origin',(0.,-1.,0.));
#9746=CARTESIAN_POINT('Origin',(1.,1.,0.));
#9747=CARTESIAN_POINT('',(1.,1.,0.));
#9748=CARTESIAN_POINT('Origin',(3.8,-1.9,0.));
#9749=CARTESIAN_POINT('Origin',(15.2,-1.9,0.));
#9750=CARTESIAN_POINT('',(15.2,-1.9,0.));
#9751=CARTESIAN_POINT('Origin',(15.2,-3.1,0.));
#9752=CARTESIAN_POINT('',(15.2,-3.1,0.));
#9753=CARTESIAN_POINT('Origin',(3.8,-3.1,0.));
#9754=CARTESIAN_POINT('',(0.,0.,0.));
#9755=CARTESIAN_POINT('Origin',(0.,0.,0.75));
#9756=CARTESIAN_POINT('',(-0.3,-3.67394039744206E-17,0.7));
#9757=CARTESIAN_POINT('Origin',(0.,0.,0.7));
#9758=CARTESIAN_POINT('',(-0.3,-3.67394039744206E-17,0.8));
#9759=CARTESIAN_POINT('',(-0.3,-3.67394039744206E-17,0.75));
#9760=CARTESIAN_POINT('Origin',(0.,0.,0.8));
#9761=CARTESIAN_POINT('Origin',(0.7,0.,0.7));
#9762=CARTESIAN_POINT('',(-0.4,4.89858719658941E-17,0.7));
#9763=CARTESIAN_POINT('Origin',(0.,0.,0.7));
#9764=CARTESIAN_POINT('Origin',(0.3,0.,0.8));
#9765=CARTESIAN_POINT('',(-0.4,-4.89858719658941E-17,0.8));
#9766=CARTESIAN_POINT('Origin',(0.,0.,0.8));
#9767=CARTESIAN_POINT('Origin',(0.,0.,-0.7));
#9768=CARTESIAN_POINT('',(-0.4,-4.89858719658941E-17,0.9));
#9769=CARTESIAN_POINT('Origin',(0.,0.,0.9));
#9770=CARTESIAN_POINT('',(-0.4,-4.89858719658941E-17,-0.7));
#9771=CARTESIAN_POINT('Origin',(0.,0.,-0.7));
#9772=CARTESIAN_POINT('',(-0.6,-7.34788079488412E-17,-0.7));
#9773=CARTESIAN_POINT('Origin',(0.,0.,-0.7));
#9774=CARTESIAN_POINT('',(-0.4,-4.89858719658941E-17,-0.7));
#9775=CARTESIAN_POINT('Origin',(0.,0.,-0.7));
#9776=CARTESIAN_POINT('Origin',(0.,0.,-0.8));
#9777=CARTESIAN_POINT('',(-0.6,-7.34788079488412E-17,-0.8));
#9778=CARTESIAN_POINT('',(-0.6,-7.34788079488412E-17,-0.8));
#9779=CARTESIAN_POINT('Origin',(0.,0.,-0.8));
#9780=CARTESIAN_POINT('Origin',(0.,0.,-0.8));
#9781=CARTESIAN_POINT('Origin',(0.,0.,-0.7));
#9782=CARTESIAN_POINT('',(-0.4,-4.89858719658941E-17,-0.7));
#9783=CARTESIAN_POINT('Origin',(0.,0.,0.9));
#9784=CARTESIAN_POINT('',(0.,0.,0.));
#9785=CARTESIAN_POINT('Origin',(-0.1,0.,0.1));
#9786=CARTESIAN_POINT('',(-0.1,0.282842712474619,0.));
#9787=CARTESIAN_POINT('',(-0.1,0.282842712474619,0.1));
#9788=CARTESIAN_POINT('',(-0.1,0.282842712474619,0.));
#9789=CARTESIAN_POINT('',(-0.1,0.591607978309962,0.));
#9790=CARTESIAN_POINT('',(-0.1,0.,0.));
#9791=CARTESIAN_POINT('',(-0.1,0.591607978309962,0.1));
#9792=CARTESIAN_POINT('',(-0.1,0.591607978309962,0.));
#9793=CARTESIAN_POINT('',(-0.1,0.,0.1));
#9794=CARTESIAN_POINT('Origin',(0.1,1.2,0.1));
#9795=CARTESIAN_POINT('',(0.1,0.282842712474619,0.1));
#9796=CARTESIAN_POINT('',(0.1,0.282842712474619,0.));
#9797=CARTESIAN_POINT('',(0.1,0.282842712474619,0.));
#9798=CARTESIAN_POINT('',(0.1,0.591607978309962,0.1));
#9799=CARTESIAN_POINT('',(0.1,0.6,0.1));
#9800=CARTESIAN_POINT('',(0.1,0.591607978309962,0.));
#9801=CARTESIAN_POINT('',(0.1,0.591607978309962,0.));
#9802=CARTESIAN_POINT('',(0.1,0.6,0.));
#9803=CARTESIAN_POINT('Origin',(0.,0.,0.));
#9804=CARTESIAN_POINT('Origin',(0.,0.,0.));
#9805=CARTESIAN_POINT('Origin',(0.,0.,0.));
#9806=CARTESIAN_POINT('Origin',(0.,0.,0.));
#9807=CARTESIAN_POINT('Origin',(0.,0.,0.1));
#9808=CARTESIAN_POINT('Origin',(0.,0.,0.));
#9809=CARTESIAN_POINT('Origin',(0.,0.,0.1));
#9810=CARTESIAN_POINT('Origin',(0.,0.,0.1));
#9811=CARTESIAN_POINT('',(0.,0.,0.));
#9812=CARTESIAN_POINT('',(0.,0.,0.));
#9813=CARTESIAN_POINT('Origin',(9.,-1.,0.8));
#9814=CARTESIAN_POINT('',(8.85,-1.,0.9));
#9815=CARTESIAN_POINT('Origin',(9.,-1.,0.9));
#9816=CARTESIAN_POINT('',(8.85,-1.,0.7));
#9817=CARTESIAN_POINT('',(8.85,-1.,0.8));
#9818=CARTESIAN_POINT('Origin',(9.,-1.,0.7));
#9819=CARTESIAN_POINT('Origin',(3.,-1.,0.8));
#9820=CARTESIAN_POINT('',(2.85,-1.,0.9));
#9821=CARTESIAN_POINT('Origin',(3.,-1.,0.9));
#9822=CARTESIAN_POINT('',(2.85,-1.,0.7));
#9823=CARTESIAN_POINT('',(2.85,-1.,0.8));
#9824=CARTESIAN_POINT('Origin',(3.,-1.,0.7));
#9825=CARTESIAN_POINT('Origin',(3.,1.,0.8));
#9826=CARTESIAN_POINT('',(2.85,1.,0.9));
#9827=CARTESIAN_POINT('Origin',(3.,1.,0.9));
#9828=CARTESIAN_POINT('',(2.85,1.,0.7));
#9829=CARTESIAN_POINT('',(2.85,1.,0.8));
#9830=CARTESIAN_POINT('Origin',(3.,1.,0.7));
#9831=CARTESIAN_POINT('Origin',(9.,1.,0.8));
#9832=CARTESIAN_POINT('',(8.85,1.,0.9));
#9833=CARTESIAN_POINT('Origin',(9.,1.,0.9));
#9834=CARTESIAN_POINT('',(8.85,1.,0.7));
#9835=CARTESIAN_POINT('',(8.85,1.,0.8));
#9836=CARTESIAN_POINT('Origin',(9.,1.,0.7));
#9837=CARTESIAN_POINT('Origin',(2.,0.,0.75));
#9838=CARTESIAN_POINT('',(1.7,3.67394039744206E-17,0.9));
#9839=CARTESIAN_POINT('Origin',(2.,0.,0.9));
#9840=CARTESIAN_POINT('',(1.7,3.67394039744206E-17,0.6));
#9841=CARTESIAN_POINT('',(1.7,3.67394039744206E-17,0.75));
#9842=CARTESIAN_POINT('Origin',(2.,0.,0.6));
#9843=CARTESIAN_POINT('Origin',(2.,0.,0.6));
#9844=CARTESIAN_POINT('',(1.83,-2.0818995585505E-17,0.6));
#9845=CARTESIAN_POINT('Origin',(2.,0.,0.6));
#9846=CARTESIAN_POINT('Origin',(10.,0.,0.75));
#9847=CARTESIAN_POINT('',(9.7,3.67394039744206E-17,0.9));
#9848=CARTESIAN_POINT('Origin',(10.,0.,0.9));
#9849=CARTESIAN_POINT('',(9.7,3.67394039744206E-17,0.6));
#9850=CARTESIAN_POINT('',(9.7,3.67394039744206E-17,0.75));
#9851=CARTESIAN_POINT('Origin',(10.,0.,0.6));
#9852=CARTESIAN_POINT('Origin',(10.,0.,0.6));
#9853=CARTESIAN_POINT('',(9.83,-2.0818995585505E-17,0.6));
#9854=CARTESIAN_POINT('Origin',(10.,0.,0.6));
#9855=CARTESIAN_POINT('Origin',(2.,0.,0.45));
#9856=CARTESIAN_POINT('',(1.83,-2.0818995585505E-17,0.32));
#9857=CARTESIAN_POINT('',(1.83,2.0818995585505E-17,0.45));
#9858=CARTESIAN_POINT('Origin',(2.,0.,0.32));
#9859=CARTESIAN_POINT('Origin',(10.,0.,0.45));
#9860=CARTESIAN_POINT('',(9.83,-2.0818995585505E-17,0.32));
#9861=CARTESIAN_POINT('',(9.83,2.0818995585505E-17,0.45));
#9862=CARTESIAN_POINT('Origin',(10.,0.,0.32));
#9863=CARTESIAN_POINT('Origin',(11.2,-0.62,0.32));
#9864=CARTESIAN_POINT('',(0.200274469199584,-0.62,0.));
#9865=CARTESIAN_POINT('',(0.217044958570157,-0.62,0.32));
#9866=CARTESIAN_POINT('',(0.223426876981161,-0.62,0.441774257530303));
#9867=CARTESIAN_POINT('',(0.,-0.62,0.));
#9868=CARTESIAN_POINT('',(8.63987299740311,-0.62,0.));
#9869=CARTESIAN_POINT('',(0.0167704893705732,-0.62,0.32));
#9870=CARTESIAN_POINT('',(0.0237009700302462,-0.62,0.452241448778892));
#9871=CARTESIAN_POINT('',(-0.1,-0.62,0.32));
#9872=CARTESIAN_POINT('Origin',(11.2,-0.62,0.32));
#9873=CARTESIAN_POINT('',(0.9,-0.62,0.32));
#9874=CARTESIAN_POINT('',(0.9,-0.62,0.));
#9875=CARTESIAN_POINT('',(0.9,-0.62,0.16));
#9876=CARTESIAN_POINT('',(1.1,-0.62,0.32));
#9877=CARTESIAN_POINT('',(-0.1,-0.62,0.32));
#9878=CARTESIAN_POINT('',(1.1,-0.62,0.));
#9879=CARTESIAN_POINT('',(1.1,-0.62,0.16));
#9880=CARTESIAN_POINT('',(8.63987299740311,-0.62,0.));
#9881=CARTESIAN_POINT('Origin',(11.2,-0.62,0.32));
#9882=CARTESIAN_POINT('',(3.9,-0.62,0.32));
#9883=CARTESIAN_POINT('',(3.9,-0.62,0.));
#9884=CARTESIAN_POINT('',(3.9,-0.62,0.16));
#9885=CARTESIAN_POINT('',(4.1,-0.62,0.32));
#9886=CARTESIAN_POINT('',(-0.1,-0.62,0.32));
#9887=CARTESIAN_POINT('',(4.1,-0.62,0.));
#9888=CARTESIAN_POINT('',(4.1,-0.62,0.16));
#9889=CARTESIAN_POINT('',(8.63987299740311,-0.62,0.));
#9890=CARTESIAN_POINT('Origin',(11.2,-0.62,0.32));
#9891=CARTESIAN_POINT('',(7.9,-0.62,0.32));
#9892=CARTESIAN_POINT('',(7.9,-0.62,0.));
#9893=CARTESIAN_POINT('',(7.9,-0.62,0.16));
#9894=CARTESIAN_POINT('',(8.1,-0.62,0.32));
#9895=CARTESIAN_POINT('',(-0.1,-0.62,0.32));
#9896=CARTESIAN_POINT('',(8.1,-0.62,0.));
#9897=CARTESIAN_POINT('',(8.1,-0.62,0.16));
#9898=CARTESIAN_POINT('',(8.63987299740311,-0.62,0.));
#9899=CARTESIAN_POINT('Origin',(-0.0999999999999996,0.62,0.32));
#9900=CARTESIAN_POINT('',(0.217044958570158,0.62,0.32));
#9901=CARTESIAN_POINT('',(0.200274469199586,0.62,0.));
#9902=CARTESIAN_POINT('',(0.207951231396534,0.62,0.146481348799182));
#9903=CARTESIAN_POINT('',(0.0167704893705736,0.62,0.32));
#9904=CARTESIAN_POINT('',(11.2,0.62,0.32));
#9905=CARTESIAN_POINT('',(0.,0.62,0.));
#9906=CARTESIAN_POINT('',(0.00822532444561912,0.62,0.156948540047771));
#9907=CARTESIAN_POINT('',(2.98987299740311,0.62,0.));
#9908=CARTESIAN_POINT('Origin',(-0.0999999999999996,0.62,0.32));
#9909=CARTESIAN_POINT('',(0.9,0.62,0.));
#9910=CARTESIAN_POINT('',(0.9,0.62,0.32));
#9911=CARTESIAN_POINT('',(0.9,0.62,0.16));
#9912=CARTESIAN_POINT('',(1.1,0.62,0.));
#9913=CARTESIAN_POINT('',(2.98987299740311,0.62,0.));
#9914=CARTESIAN_POINT('',(1.1,0.62,0.32));
#9915=CARTESIAN_POINT('',(1.1,0.62,0.16));
#9916=CARTESIAN_POINT('',(11.2,0.62,0.32));
#9917=CARTESIAN_POINT('Origin',(-0.0999999999999996,0.62,0.32));
#9918=CARTESIAN_POINT('',(3.9,0.62,0.));
#9919=CARTESIAN_POINT('',(3.9,0.62,0.32));
#9920=CARTESIAN_POINT('',(3.9,0.62,0.16));
#9921=CARTESIAN_POINT('',(4.1,0.62,0.));
#9922=CARTESIAN_POINT('',(2.98987299740311,0.62,0.));
#9923=CARTESIAN_POINT('',(4.1,0.62,0.32));
#9924=CARTESIAN_POINT('',(4.1,0.62,0.16));
#9925=CARTESIAN_POINT('',(11.2,0.62,0.32));
#9926=CARTESIAN_POINT('Origin',(5.55,0.,0.32));
#9927=CARTESIAN_POINT('',(1.6,-4.89858719658941E-17,0.32));
#9928=CARTESIAN_POINT('Origin',(2.,0.,0.32));
#9929=CARTESIAN_POINT('Origin',(5.55,0.,0.32));
#9930=CARTESIAN_POINT('',(9.6,-4.89858719658942E-17,0.32));
#9931=CARTESIAN_POINT('Origin',(10.,0.,0.32));
#9932=CARTESIAN_POINT('Origin',(5.55,0.,0.32));
#9933=CARTESIAN_POINT('',(0.217044958570157,-0.7,0.32));
#9934=CARTESIAN_POINT('',(0.0167704893705731,-0.7,0.32));
#9935=CARTESIAN_POINT('Origin',(5.55,0.,0.32));
#9936=CARTESIAN_POINT('',(0.9,0.724814814814815,0.32));
#9937=CARTESIAN_POINT('',(1.1,-0.724814814814815,0.32));
#9938=CARTESIAN_POINT('Origin',(5.55,0.,0.32));
#9939=CARTESIAN_POINT('',(3.9,0.883148148148148,0.32));
#9940=CARTESIAN_POINT('',(4.1,-0.883148148148148,0.32));
#9941=CARTESIAN_POINT('Origin',(5.55,0.,0.32));
#9942=CARTESIAN_POINT('',(7.9,0.62,0.32));
#9943=CARTESIAN_POINT('',(7.9,0.886851851851852,0.32));
#9944=CARTESIAN_POINT('',(8.1,0.62,0.32));
#9945=CARTESIAN_POINT('',(11.2,0.62,0.32));
#9946=CARTESIAN_POINT('',(8.1,-0.886851851851852,0.32));
#9947=CARTESIAN_POINT('Origin',(-0.0999999999999996,0.62,0.32));
#9948=CARTESIAN_POINT('',(7.9,0.62,0.));
#9949=CARTESIAN_POINT('',(7.9,0.62,0.16));
#9950=CARTESIAN_POINT('',(8.1,0.62,0.));
#9951=CARTESIAN_POINT('',(2.98987299740311,0.62,0.));
#9952=CARTESIAN_POINT('',(8.1,0.62,0.16));
#9953=CARTESIAN_POINT('Origin',(11.2,1.53779953703704,0.));
#9954=CARTESIAN_POINT('',(11.2,1.47592264243751,0.));
#9955=CARTESIAN_POINT('',(11.2,-1.47592264243751,0.));
#9956=CARTESIAN_POINT('',(11.2,1.53779953703704,0.));
#9957=CARTESIAN_POINT('',(11.2,-1.44160695250311,0.605635447211793));
#9958=CARTESIAN_POINT('Ctrl Pts',(11.2,-1.44160695250311,0.605635447211793));
#9959=CARTESIAN_POINT('Ctrl Pts',(11.2,-1.44733381480461,0.504614841520655));
#9960=CARTESIAN_POINT('Ctrl Pts',(11.2,-1.45305922122436,0.403593539811385));
#9961=CARTESIAN_POINT('Ctrl Pts',(11.2,-1.46449774781658,0.201715464978033));
#9962=CARTESIAN_POINT('Ctrl Pts',(11.2,-1.47021094199039,0.100857470386242));
#9963=CARTESIAN_POINT('Ctrl Pts',(11.2,-1.47592264243751,0.));
#9964=CARTESIAN_POINT('',(11.2,-1.3413305091784,0.7));
#9965=CARTESIAN_POINT('Ctrl Pts',(11.2,-1.34133050917871,0.7));
#9966=CARTESIAN_POINT('Ctrl Pts',(11.2,-1.34927184579059,0.7));
#9967=CARTESIAN_POINT('Ctrl Pts',(11.1999981201149,-1.35715077597425,0.699006225306896));
#9968=CARTESIAN_POINT('Ctrl Pts',(11.1999964866412,-1.36482619101963,0.697118463987577));
#9969=CARTESIAN_POINT('Ctrl Pts',(11.1999955714568,-1.36912648693643,0.696060810134936));
#9970=CARTESIAN_POINT('Ctrl Pts',(11.1999947385598,-1.37336294684024,0.694721504600825));
#9971=CARTESIAN_POINT('Ctrl Pts',(11.1999942054834,-1.37750904339755,0.693111246644731));
#9972=CARTESIAN_POINT('Ctrl Pts',(11.1999932489192,-1.38494889279378,0.690221763364053));
#9973=CARTESIAN_POINT('Ctrl Pts',(11.1999934335488,-1.39201911070639,0.686493604183975));
#9974=CARTESIAN_POINT('Ctrl Pts',(11.1999946360439,-1.39857284316731,0.682006025455124));
#9975=CARTESIAN_POINT('Ctrl Pts',(11.1999952980149,-1.40218065925828,0.679535622697003));
#9976=CARTESIAN_POINT('Ctrl Pts',(11.1999962427007,-1.40563167682227,0.676834205328214));
#9977=CARTESIAN_POINT('Ctrl Pts',(11.1999970766466,-1.40889738828709,0.673909521834337));
#9978=CARTESIAN_POINT('Ctrl Pts',(11.1999978839828,-1.41205889660265,0.671078159882768));
#9979=CARTESIAN_POINT('Ctrl Pts',(11.1999985961359,-1.41502771690814,0.668054510912379));
#9980=CARTESIAN_POINT('Ctrl Pts',(11.1999985943254,-1.41778154893794,0.664849526385156));
#9981=CARTESIAN_POINT('Ctrl Pts',(11.1999985909468,-1.42292039881534,0.658868793295219));
#9982=CARTESIAN_POINT('Ctrl Pts',(11.1999963776609,-1.42731355725865,0.652257958652517));
#9983=CARTESIAN_POINT('Ctrl Pts',(11.1999956369,-1.43089859237711,0.645180832176479));
#9984=CARTESIAN_POINT('Ctrl Pts',(11.1999955610412,-1.43126572346771,0.644456088045497));
#9985=CARTESIAN_POINT('Ctrl Pts',(11.1999954968237,-1.43162433912915,0.643726434786758));
#9986=CARTESIAN_POINT('Ctrl Pts',(11.1999954455063,-1.43197434355081,0.642992037678167));
#9987=CARTESIAN_POINT('Ctrl Pts',(11.1999949451572,-1.43538691836834,0.635831599341589));
#9988=CARTESIAN_POINT('Ctrl Pts',(11.1999960935741,-1.43794480573841,0.628305806294037));
#9989=CARTESIAN_POINT('Ctrl Pts',(11.1999977538348,-1.43959303921538,0.620581877990282));
#9990=CARTESIAN_POINT('Ctrl Pts',(11.1999988103007,-1.44064185190664,0.615666946856702));
#9991=CARTESIAN_POINT('Ctrl Pts',(11.1999999935832,-1.44132148083109,0.610671141596651));
#9992=CARTESIAN_POINT('Ctrl Pts',(11.1999999950647,-1.44160695392865,0.605635447210179));
#9993=CARTESIAN_POINT('',(11.2,1.34133050917871,0.7));
#9994=CARTESIAN_POINT('',(11.2,0.768899768518519,0.7));
#9995=CARTESIAN_POINT('',(11.2,1.44160695250311,0.605635447211793));
#9996=CARTESIAN_POINT('Ctrl Pts',(11.1999999950647,1.44160695392865,0.605635447210179));
#9997=CARTESIAN_POINT('Ctrl Pts',(11.1999999927383,1.44115867123275,0.613543073794128));
#9998=CARTESIAN_POINT('Ctrl Pts',(11.199997327584,1.43974095598264,0.62135504174347));
#9999=CARTESIAN_POINT('Ctrl Pts',(11.1999961426836,1.43743894790867,0.628911795513178));
#10000=CARTESIAN_POINT('Ctrl Pts',(11.1999954950047,1.43618064644969,0.633042395401645));
#10001=CARTESIAN_POINT('Ctrl Pts',(11.1999951984378,1.4346571631488,0.63709676955888));
#10002=CARTESIAN_POINT('Ctrl Pts',(11.1999953420225,1.43287614971348,0.641047046155727));
#10003=CARTESIAN_POINT('Ctrl Pts',(11.1999956050472,1.42961361303411,0.648283331988978));
#10004=CARTESIAN_POINT('Ctrl Pts',(11.1999975633633,1.42552584716917,0.655091209244077));
#10005=CARTESIAN_POINT('Ctrl Pts',(11.1999983488166,1.42067941835906,0.661308913390503));
#10006=CARTESIAN_POINT('Ctrl Pts',(11.1999985007599,1.41974189284539,0.662511707551344));
#10007=CARTESIAN_POINT('Ctrl Pts',(11.1999985958742,1.41877583892185,0.663692344451305));
#10008=CARTESIAN_POINT('Ctrl Pts',(11.1999985956185,1.41778154881703,0.664849526385225));
#10009=CARTESIAN_POINT('Ctrl Pts',(11.199998595152,1.41596832836708,0.666959801783445));
#10010=CARTESIAN_POINT('Ctrl Pts',(11.1999982799021,1.41406123008998,0.668992111776222));
#10011=CARTESIAN_POINT('Ctrl Pts',(11.1999978412043,1.41206657472189,0.670943322037058));
#10012=CARTESIAN_POINT('Ctrl Pts',(11.1999965906985,1.40638082038708,0.676505236328724));
#10013=CARTESIAN_POINT('Ctrl Pts',(11.1999945592311,1.40005057587654,0.681348449922958));
#10014=CARTESIAN_POINT('Ctrl Pts',(11.1999938793032,1.39324090595796,0.685420973467861));
#10015=CARTESIAN_POINT('Ctrl Pts',(11.1999934424014,1.38886521116801,0.68803785802621));
#10016=CARTESIAN_POINT('Ctrl Pts',(11.1999934711477,1.38429057260668,0.690335857752236));
#10017=CARTESIAN_POINT('Ctrl Pts',(11.1999939665515,1.37955471147715,0.692291686537622));
#10018=CARTESIAN_POINT('Ctrl Pts',(11.1999947349645,1.37220899016913,0.695325342464331));
#10019=CARTESIAN_POINT('Ctrl Pts',(11.1999966395725,1.36455954597093,0.697503651902993));
#10020=CARTESIAN_POINT('Ctrl Pts',(11.1999981885915,1.35675452105021,0.698758058199902));
#10021=CARTESIAN_POINT('Ctrl Pts',(11.1999991983045,1.35166689148409,0.699575730741489));
#10022=CARTESIAN_POINT('Ctrl Pts',(11.2,1.34651254223162,0.7));
#10023=CARTESIAN_POINT('Ctrl Pts',(11.2,1.34133050917871,0.7));
#10024=CARTESIAN_POINT('Ctrl Pts',(11.2,1.47592264243751,0.));
#10025=CARTESIAN_POINT('Ctrl Pts',(11.2,1.47021025951677,0.100869521536925));
#10026=CARTESIAN_POINT('Ctrl Pts',(11.2,1.4644963825062,0.20173956751342));
#10027=CARTESIAN_POINT('Ctrl Pts',(11.2,1.45305785520703,0.403617642353031));
#10028=CARTESIAN_POINT('Ctrl Pts',(11.2,1.44733313162379,0.50462689268162));
#10029=CARTESIAN_POINT('Ctrl Pts',(11.2,1.44160695250311,0.605635447211793));
#10030=CARTESIAN_POINT('Origin',(8.1,-1.7737037037037,0.));
#10031=CARTESIAN_POINT('',(8.1,1.69866351109718,0.));
#10032=CARTESIAN_POINT('',(8.1,-1.7737037037037,0.));
#10033=CARTESIAN_POINT('',(8.1,1.66641703131627,0.605314487869832));
#10034=CARTESIAN_POINT('Ctrl Pts',(8.1,1.66641703131627,0.605314487869832));
#10035=CARTESIAN_POINT('Ctrl Pts',(8.1,1.67178339996556,0.504592280948055));
#10036=CARTESIAN_POINT('Ctrl Pts',(8.1,1.67714947719849,0.403869246528492));
#10037=CARTESIAN_POINT('Ctrl Pts',(8.1,1.68789827452893,0.202098297941347));
#10038=CARTESIAN_POINT('Ctrl Pts',(8.1,1.69328107955938,0.101048748975501));
#10039=CARTESIAN_POINT('Ctrl Pts',(8.1,1.69866351109718,0.));
#10040=CARTESIAN_POINT('',(8.1,1.56644778183753,0.7));
#10041=CARTESIAN_POINT('Ctrl Pts',(8.0999999986552,1.56644778212326,0.7));
#10042=CARTESIAN_POINT('Ctrl Pts',(8.10000000155239,1.57436337254628,0.699999999341293));
#10043=CARTESIAN_POINT('Ctrl Pts',(8.09999905041684,1.58221543358893,0.699005989267703));
#10044=CARTESIAN_POINT('Ctrl Pts',(8.09999821745812,1.58986365929578,0.697118696434997));
#10045=CARTESIAN_POINT('Ctrl Pts',(8.099997748439,1.59417019217574,0.69605600700222));
#10046=CARTESIAN_POINT('Ctrl Pts',(8.09999731997616,1.59841215407948,0.694709061504878));
#10047=CARTESIAN_POINT('Ctrl Pts',(8.09999704681388,1.60256279759721,0.693088866918468));
#10048=CARTESIAN_POINT('Ctrl Pts',(8.09999655811104,1.60998853482381,0.690190246691698));
#10049=CARTESIAN_POINT('Ctrl Pts',(8.09999665589197,1.61704187682962,0.686451534538094));
#10050=CARTESIAN_POINT('Ctrl Pts',(8.09999726576867,1.62357667434142,0.681954089017224));
#10051=CARTESIAN_POINT('Ctrl Pts',(8.09999760196939,1.62717904774802,0.679474826559159));
#10052=CARTESIAN_POINT('Ctrl Pts',(8.09999808150314,1.6306235748906,0.676764109620253));
#10053=CARTESIAN_POINT('Ctrl Pts',(8.09999850764167,1.63388182210815,0.673830012183301));
#10054=CARTESIAN_POINT('Ctrl Pts',(8.09999892160867,1.637047006066,0.670979719520364));
#10055=CARTESIAN_POINT('Ctrl Pts',(8.09999928906958,1.640017230617,0.667935813742119));
#10056=CARTESIAN_POINT('Ctrl Pts',(8.09999928944056,1.64277007752663,0.664709670235875));
#10057=CARTESIAN_POINT('Ctrl Pts',(8.09999929012967,1.64788359851353,0.658716982277737));
#10058=CARTESIAN_POINT('Ctrl Pts',(8.09999816327153,1.65225000627493,0.652096887528603));
#10059=CARTESIAN_POINT('Ctrl Pts',(8.09999778355904,1.65580927004486,0.645014643130784));
#10060=CARTESIAN_POINT('Ctrl Pts',(8.09999774450894,1.65617530914943,0.644286296325024));
#10061=CARTESIAN_POINT('Ctrl Pts',(8.09999771143612,1.65653277094855,0.643553041785202));
#10062=CARTESIAN_POINT('Ctrl Pts',(8.0999976850083,1.65688156115921,0.642815048027137));
#10063=CARTESIAN_POINT('Ctrl Pts',(8.09999742811004,1.66027206465027,0.635641192980042));
#10064=CARTESIAN_POINT('Ctrl Pts',(8.09999800724182,1.66280786743682,0.628104262855387));
#10065=CARTESIAN_POINT('Ctrl Pts',(8.09999885110511,1.66443535430957,0.620372450280339));
#10066=CARTESIAN_POINT('Ctrl Pts',(8.09999939164969,1.6654778563549,0.615419764910946));
#10067=CARTESIAN_POINT('Ctrl Pts',(8.1,1.66614680274328,0.610386449940169));
#10068=CARTESIAN_POINT('Ctrl Pts',(8.1,1.66641703131627,0.605314487869832));
#10069=CARTESIAN_POINT('',(8.1,-1.56644778183827,0.7));
#10070=CARTESIAN_POINT('',(8.1,-0.886851851851852,0.7));
#10071=CARTESIAN_POINT('',(8.1,-1.66641703131627,0.605314487869832));
#10072=CARTESIAN_POINT('Ctrl Pts',(8.1,-1.66641703131627,0.605314487869832));
#10073=CARTESIAN_POINT('Ctrl Pts',(8.1,-1.66599546653325,0.613226902778437));
#10074=CARTESIAN_POINT('Ctrl Pts',(8.09999864563672,-1.66460605882141,0.621047760783158));
#10075=CARTESIAN_POINT('Ctrl Pts',(8.09999804140045,-1.66233302739118,0.628616817026045));
#10076=CARTESIAN_POINT('Ctrl Pts',(8.09999770486592,-1.66106704316887,0.632832467392296));
#10077=CARTESIAN_POINT('Ctrl Pts',(8.0999975536836,-1.65952595995304,0.636970042829054));
#10078=CARTESIAN_POINT('Ctrl Pts',(8.09999763427866,-1.65771765414013,0.640999885518982));
#10079=CARTESIAN_POINT('Ctrl Pts',(8.09999777898787,-1.65447082344915,0.64823550729937));
#10080=CARTESIAN_POINT('Ctrl Pts',(8.09999878245444,-1.65040085231772,0.655045563401426));
#10081=CARTESIAN_POINT('Ctrl Pts',(8.09999917121848,-1.64557198994432,0.661267087195486));
#10082=CARTESIAN_POINT('Ctrl Pts',(8.09999924425118,-1.6446648462537,0.662435854416292));
#10083=CARTESIAN_POINT('Ctrl Pts',(8.09999928944999,-1.64373079085321,0.663583781603691));
#10084=CARTESIAN_POINT('Ctrl Pts',(8.09999928890117,-1.64277007755202,0.664709670235858));
#10085=CARTESIAN_POINT('Ctrl Pts',(8.09999928782175,-1.64088054556816,0.666924069243459));
#10086=CARTESIAN_POINT('Ctrl Pts',(8.09999911129818,-1.63888792496677,0.66905326411728));
#10087=CARTESIAN_POINT('Ctrl Pts',(8.09999887085824,-1.63679941630975,0.671093569621172));
#10088=CARTESIAN_POINT('Ctrl Pts',(8.09999821641022,-1.6311147520694,0.676647030794692));
#10089=CARTESIAN_POINT('Ctrl Pts',(8.0999972000003,-1.62478663867955,0.681482189379454));
#10090=CARTESIAN_POINT('Ctrl Pts',(8.09999686812141,-1.6179789612855,0.685544965666037));
#10091=CARTESIAN_POINT('Ctrl Pts',(8.09999665686968,-1.61364565292072,0.68813105508359));
#10092=CARTESIAN_POINT('Ctrl Pts',(8.09999667786582,-1.6091170759025,0.690403516124292));
#10093=CARTESIAN_POINT('Ctrl Pts',(8.0999969341683,-1.60442977212996,0.692339085768374));
#10094=CARTESIAN_POINT('Ctrl Pts',(8.09999733452329,-1.59710801128849,0.695362524980696));
#10095=CARTESIAN_POINT('Ctrl Pts',(8.09999831212369,-1.58948382509795,0.697531565976904));
#10096=CARTESIAN_POINT('Ctrl Pts',(8.09999909563861,-1.58170429192971,0.698776637084609));
#10097=CARTESIAN_POINT('Ctrl Pts',(8.09999960249138,-1.57667174192468,0.69958206878261));
#10098=CARTESIAN_POINT('Ctrl Pts',(8.1000000005313,-1.5715735875011,0.699999999573449));
#10099=CARTESIAN_POINT('Ctrl Pts',(8.0999999986552,-1.56644778212326,0.7));
#10100=CARTESIAN_POINT('',(8.1,-1.69866351109718,0.));
#10101=CARTESIAN_POINT('Ctrl Pts',(8.1,-1.69866351109718,0.));
#10102=CARTESIAN_POINT('Ctrl Pts',(8.1,-1.69328105674055,0.101049177371948));
#10103=CARTESIAN_POINT('Ctrl Pts',(8.1,-1.68789822886868,0.202099155105557));
#10104=CARTESIAN_POINT('Ctrl Pts',(8.1,-1.67714943151225,0.403870104074094));
#10105=CARTESIAN_POINT('Ctrl Pts',(8.1,-1.67178337712185,0.50459270970527));
#10106=CARTESIAN_POINT('Ctrl Pts',(8.1,-1.66641703131627,0.605314487869832));
#10107=CARTESIAN_POINT('',(8.1,-1.7737037037037,0.));
#10108=CARTESIAN_POINT('Origin',(4.1,-1.7662962962963,0.));
#10109=CARTESIAN_POINT('',(4.1,1.70113889814581,0.));
#10110=CARTESIAN_POINT('',(4.1,-1.7662962962963,0.));
#10111=CARTESIAN_POINT('',(4.1,1.66887738702937,0.605315322680072));
#10112=CARTESIAN_POINT('Ctrl Pts',(4.1,1.66887738702937,0.605315322680072));
#10113=CARTESIAN_POINT('Ctrl Pts',(4.1,1.67424235111642,0.50466767694528));
#10114=CARTESIAN_POINT('Ctrl Pts',(4.1,1.67960699363804,0.404019058341251));
#10115=CARTESIAN_POINT('Ctrl Pts',(4.1,1.69036079691899,0.202247931921761));
#10116=CARTESIAN_POINT('Ctrl Pts',(4.1,1.6957500571643,0.101123491803998));
#10117=CARTESIAN_POINT('Ctrl Pts',(4.1,1.70113889814581,0.));
#10118=CARTESIAN_POINT('',(4.1,1.56887583540973,0.7));
#10119=CARTESIAN_POINT('Ctrl Pts',(4.1,1.56887583540973,0.7));
#10120=CARTESIAN_POINT('Ctrl Pts',(4.1,1.57679416129392,0.7));
#10121=CARTESIAN_POINT('Ctrl Pts',(4.10000107724674,1.58464912207822,0.699006028000541));
#10122=CARTESIAN_POINT('Ctrl Pts',(4.10000201939527,1.59230028572239,0.697118705459362));
#10123=CARTESIAN_POINT('Ctrl Pts',(4.10000255022779,1.59661116283941,0.696055335763773));
#10124=CARTESIAN_POINT('Ctrl Pts',(4.10000303435977,1.60085740028891,0.694707333985525));
#10125=CARTESIAN_POINT('Ctrl Pts',(4.10000334030352,1.60501217339351,0.693085708041268));
#10126=CARTESIAN_POINT('Ctrl Pts',(4.10000388718746,1.61243895913315,0.690187001388783));
#10127=CARTESIAN_POINT('Ctrl Pts',(4.10000376557609,1.61949349263125,0.686448444730844));
#10128=CARTESIAN_POINT('Ctrl Pts',(4.10000306534783,1.6260295229635,0.681951159450519));
#10129=CARTESIAN_POINT('Ctrl Pts',(4.10000267892397,1.62963645835533,0.679469313954069));
#10130=CARTESIAN_POINT('Ctrl Pts',(4.10000213012555,1.63308521926452,0.676755517937216));
#10131=CARTESIAN_POINT('Ctrl Pts',(4.1000016436875,1.63634725251217,0.673817835781739));
#10132=CARTESIAN_POINT('Ctrl Pts',(4.10000117237165,1.63950787692018,0.67097147916344));
#10133=CARTESIAN_POINT('Ctrl Pts',(4.10000075597222,1.64247408874941,0.667932078875657));
#10134=CARTESIAN_POINT('Ctrl Pts',(4.10000075698646,1.64522354659423,0.664710927554201));
#10135=CARTESIAN_POINT('Ctrl Pts',(4.1000007588733,1.65033845220459,0.658718515269377));
#10136=CARTESIAN_POINT('Ctrl Pts',(4.10000204656096,1.65470614797426,0.652098486008568));
#10137=CARTESIAN_POINT('Ctrl Pts',(4.10000248678323,1.65826650381873,0.645016049251367));
#10138=CARTESIAN_POINT('Ctrl Pts',(4.10000253228732,1.65863452415637,0.644283964909082));
#10139=CARTESIAN_POINT('Ctrl Pts',(4.10000257095464,1.65899387729575,0.643546919913709));
#10140=CARTESIAN_POINT('Ctrl Pts',(4.10000260201855,1.65934446736461,0.642805085364403));
#10141=CARTESIAN_POINT('Ctrl Pts',(4.10000290242009,1.66273482600052,0.635631222228741));
#10142=CARTESIAN_POINT('Ctrl Pts',(4.10000225562543,1.66527033938482,0.628094305374488));
#10143=CARTESIAN_POINT('Ctrl Pts',(4.10000130084992,1.66689736875237,0.62036252267401));
#10144=CARTESIAN_POINT('Ctrl Pts',(4.10000068968835,1.66793884687677,0.615413329558163));
#10145=CARTESIAN_POINT('Ctrl Pts',(4.09999999901039,1.66860722297681,0.610383627857512));
#10146=CARTESIAN_POINT('Ctrl Pts',(4.09999999630223,1.66887738567036,0.60531532268817));
#10147=CARTESIAN_POINT('',(4.1,-1.56887583540947,0.7));
#10148=CARTESIAN_POINT('',(4.1,-0.883148148148148,0.7));
#10149=CARTESIAN_POINT('',(4.1,-1.66887738702937,0.605315322680072));
#10150=CARTESIAN_POINT('Ctrl Pts',(4.09999999630223,-1.66887738567036,0.60531532268817));
#10151=CARTESIAN_POINT('Ctrl Pts',(4.10000000053001,-1.66845562780346,0.613227583070809));
#10152=CARTESIAN_POINT('Ctrl Pts',(4.10000153668442,-1.66706589531621,0.621048261667561));
#10153=CARTESIAN_POINT('Ctrl Pts',(4.10000221487211,-1.66479240287642,0.628617079688242));
#10154=CARTESIAN_POINT('Ctrl Pts',(4.10000259231836,-1.6635270876889,0.632829515245766));
#10155=CARTESIAN_POINT('Ctrl Pts',(4.10000275805793,-1.66198703315979,0.636963972243471));
#10156=CARTESIAN_POINT('Ctrl Pts',(4.10000266178038,-1.66018010017296,0.640990858692597));
#10157=CARTESIAN_POINT('Ctrl Pts',(4.10000248876893,-1.65693302887506,0.648227201990446));
#10158=CARTESIAN_POINT('Ctrl Pts',(4.10000134097948,-1.65286254930452,0.655037795911226));
#10159=CARTESIAN_POINT('Ctrl Pts',(4.100000893742,-1.6480330317196,0.661259713776781));
#10160=CARTESIAN_POINT('Ctrl Pts',(4.10000080951506,-1.647123502594,0.662431469633614));
#10161=CARTESIAN_POINT('Ctrl Pts',(4.10000075717637,-1.6461869221106,0.663582276554164));
#10162=CARTESIAN_POINT('Ctrl Pts',(4.10000075728519,-1.64522354661022,0.66471092755419));
#10163=CARTESIAN_POINT('Ctrl Pts',(4.10000075749815,-1.64333815989002,0.666919768869269));
#10164=CARTESIAN_POINT('Ctrl Pts',(4.1000009568795,-1.64135017761634,0.669043797975229));
#10165=CARTESIAN_POINT('Ctrl Pts',(4.10000122972053,-1.63926675509047,0.671079366787198));
#10166=CARTESIAN_POINT('Ctrl Pts',(4.10000197419082,-1.6335819569127,0.676633591976433));
#10167=CARTESIAN_POINT('Ctrl Pts',(4.10000313643093,-1.62725355063421,0.681469444454218));
#10168=CARTESIAN_POINT('Ctrl Pts',(4.1000035230587,-1.62044557755217,0.685533082105531));
#10169=CARTESIAN_POINT('Ctrl Pts',(4.10000376939409,-1.61610795658125,0.688122181633714));
#10170=CARTESIAN_POINT('Ctrl Pts',(4.10000375220654,-1.61157469281532,0.690397125746379));
#10171=CARTESIAN_POINT('Ctrl Pts',(4.10000346632868,-1.60688245467732,0.692334655286926));
#10172=CARTESIAN_POINT('Ctrl Pts',(4.10000302008581,-1.59955807566073,0.695359054367588));
#10173=CARTESIAN_POINT('Ctrl Pts',(4.1000019139068,-1.59193114173487,0.69752894708864));
#10174=CARTESIAN_POINT('Ctrl Pts',(4.10000102635309,-1.58414888227482,0.698774888159427));
#10175=CARTESIAN_POINT('Ctrl Pts',(4.10000045177616,-1.57911086966871,0.699581474839467));
#10176=CARTESIAN_POINT('Ctrl Pts',(4.1,-1.57400716417114,0.7));
#10177=CARTESIAN_POINT('Ctrl Pts',(4.1,-1.56887583540973,0.7));
#10178=CARTESIAN_POINT('',(4.1,-1.70113889814582,0.));
#10179=CARTESIAN_POINT('Ctrl Pts',(4.1,-1.70113889814582,0.));
#10180=CARTESIAN_POINT('Ctrl Pts',(4.1,-1.69575004793467,0.101123665001254));
#10181=CARTESIAN_POINT('Ctrl Pts',(4.1,-1.69036077845691,0.202248278345555));
#10182=CARTESIAN_POINT('Ctrl Pts',(4.1,-1.67960697517202,0.404019404791024));
#10183=CARTESIAN_POINT('Ctrl Pts',(4.1,-1.67424234188296,0.504667850166609));
#10184=CARTESIAN_POINT('Ctrl Pts',(4.1,-1.66887738702937,0.605315322680072));
#10185=CARTESIAN_POINT('',(4.1,-1.7662962962963,0.));
#10186=CARTESIAN_POINT('Origin',(1.1,-1.44962962962963,0.));
#10187=CARTESIAN_POINT('',(1.1,1.39262953588351,0.));
#10188=CARTESIAN_POINT('',(1.1,-1.44962962962963,0.));
#10189=CARTESIAN_POINT('',(1.10000000000005,1.35674377243284,0.605845626926786));
#10190=CARTESIAN_POINT('Ctrl Pts',(1.10000000000005,1.35674377243284,0.605845626926786));
#10191=CARTESIAN_POINT('Ctrl Pts',(1.10000000000005,1.36273568520883,0.504787121979256));
#10192=CARTESIAN_POINT('Ctrl Pts',(1.1,1.36872466312622,0.403727404115485));
#10193=CARTESIAN_POINT('Ctrl Pts',(1.1,1.38068651056748,0.201779555185378));
#10194=CARTESIAN_POINT('Ctrl Pts',(1.1,1.38665951284069,0.10088935150083));
#10195=CARTESIAN_POINT('Ctrl Pts',(1.1,1.39262953588351,0.));
#10196=CARTESIAN_POINT('',(1.1,1.25565664448622,0.7));
#10197=CARTESIAN_POINT('Ctrl Pts',(1.1,1.25565664448621,0.7));
#10198=CARTESIAN_POINT('Ctrl Pts',(1.1,1.26365753466764,0.700000000000001));
#10199=CARTESIAN_POINT('Ctrl Pts',(1.10000312127109,1.27160078819195,0.699008097631352));
#10200=CARTESIAN_POINT('Ctrl Pts',(1.10000579554281,1.27934333527045,0.697120485426804));
#10201=CARTESIAN_POINT('Ctrl Pts',(1.10000709386889,1.28310224676699,0.696204072889075));
#10202=CARTESIAN_POINT('Ctrl Pts',(1.10000828779753,1.28681383019745,0.695075712339665));
#10203=CARTESIAN_POINT('Ctrl Pts',(1.10000913303706,1.29046059826345,0.693742188764313));
#10204=CARTESIAN_POINT('Ctrl Pts',(1.10001087659788,1.29798315455626,0.69099139518989));
#10205=CARTESIAN_POINT('Ctrl Pts',(1.10001086910546,1.30515375246939,0.687398976275641));
#10206=CARTESIAN_POINT('Ctrl Pts',(1.10000899624477,1.31182501206943,0.683041610144935));
#10207=CARTESIAN_POINT('Ctrl Pts',(1.10000779407289,1.31610723164143,0.680244657298552));
#10208=CARTESIAN_POINT('Ctrl Pts',(1.10000585478529,1.32018349952736,0.677131483611404));
#10209=CARTESIAN_POINT('Ctrl Pts',(1.10000422180804,1.32400796947387,0.673713330684339));
#10210=CARTESIAN_POINT('Ctrl Pts',(1.10000291018178,1.3270798280974,0.670967830603965));
#10211=CARTESIAN_POINT('Ctrl Pts',(1.10000180047651,1.32997084712789,0.668041731908725));
#10212=CARTESIAN_POINT('Ctrl Pts',(1.10000182449184,1.33266034096938,0.664944387470286));
#10213=CARTESIAN_POINT('Ctrl Pts',(1.10000187074845,1.33784065079383,0.65897850512594));
#10214=CARTESIAN_POINT('Ctrl Pts',(1.10000564109429,1.34227630326151,0.652378581761819));
#10215=CARTESIAN_POINT('Ctrl Pts',(1.10000696187003,1.34590032739451,0.645305437365917));
#10216=CARTESIAN_POINT('Ctrl Pts',(1.100007110355,1.34630774940504,0.644510256482779));
#10217=CARTESIAN_POINT('Ctrl Pts',(1.10000723579819,1.34670486410349,0.643709073603569));
#10218=CARTESIAN_POINT('Ctrl Pts',(1.10000733566964,1.34709153749004,0.642902104572485));
#10219=CARTESIAN_POINT('Ctrl Pts',(1.10000822022419,1.35051627708745,0.63575483535061));
#10220=CARTESIAN_POINT('Ctrl Pts',(1.10000635568239,1.35308446649167,0.628241602461225));
#10221=CARTESIAN_POINT('Ctrl Pts',(1.10000361780323,1.35473867947858,0.620527690691125));
#10222=CARTESIAN_POINT('Ctrl Pts',(1.1000019043033,1.35577396762308,0.615699943921843));
#10223=CARTESIAN_POINT('Ctrl Pts',(1.09999998677418,1.35645041192828,0.610792997969602));
#10224=CARTESIAN_POINT('Ctrl Pts',(1.09999997754868,1.35674374570294,0.605845627052288));
#10225=CARTESIAN_POINT('',(1.1,-1.25565664448622,0.7));
#10226=CARTESIAN_POINT('',(1.1,-0.724814814814815,0.7));
#10227=CARTESIAN_POINT('',(1.10000000000005,-1.35674377243284,0.605845626926786));
#10228=CARTESIAN_POINT('Ctrl Pts',(1.09999997754868,-1.35674374570294,0.605845627052288));
#10229=CARTESIAN_POINT('Ctrl Pts',(1.09999999227748,-1.35627542940044,0.613744255356351));
#10230=CARTESIAN_POINT('Ctrl Pts',(1.1000044245081,-1.35483313756702,0.621542702113576));
#10231=CARTESIAN_POINT('Ctrl Pts',(1.10000632213307,-1.3525036790266,0.629082464357584));
#10232=CARTESIAN_POINT('Ctrl Pts',(1.1000073336739,-1.3512619466217,0.633101581650771));
#10233=CARTESIAN_POINT('Ctrl Pts',(1.10000777634458,-1.34976719347553,0.637047225321331));
#10234=CARTESIAN_POINT('Ctrl Pts',(1.10000752568741,-1.34802684471036,0.640893844816285));
#10235=CARTESIAN_POINT('Ctrl Pts',(1.10000705344834,-1.3447480208661,0.648140890909733));
#10236=CARTESIAN_POINT('Ctrl Pts',(1.10000374385205,-1.34063788586045,0.654954534019122));
#10237=CARTESIAN_POINT('Ctrl Pts',(1.10000230512149,-1.33576793982513,0.661175616324976));
#10238=CARTESIAN_POINT('Ctrl Pts',(1.10000200863552,-1.33476436716076,0.662457623989879));
#10239=CARTESIAN_POINT('Ctrl Pts',(1.10000181701501,-1.33372836971272,0.663714393476354));
#10240=CARTESIAN_POINT('Ctrl Pts',(1.10000180919237,-1.33266033853372,0.664944387472089));
#10241=CARTESIAN_POINT('Ctrl Pts',(1.10000179685332,-1.33097567746633,0.666884520904953));
#10242=CARTESIAN_POINT('Ctrl Pts',(1.10000223926429,-1.32921133126375,0.668758058859172));
#10243=CARTESIAN_POINT('Ctrl Pts',(1.10000288715521,-1.32737234926393,0.670562692084704));
#10244=CARTESIAN_POINT('Ctrl Pts',(1.10000489069569,-1.32168547392559,0.676143347135183));
#10245=CARTESIAN_POINT('Ctrl Pts',(1.10000845923633,-1.31535192007569,0.681005160308095));
#10246=CARTESIAN_POINT('Ctrl Pts',(1.1000097672184,-1.30853956043085,0.685101187995272));
#10247=CARTESIAN_POINT('Ctrl Pts',(1.10001062829021,-1.30405484229164,0.687797688271992));
#10248=CARTESIAN_POINT('Ctrl Pts',(1.10001067755751,-1.29936155475819,0.690161668140197));
#10249=CARTESIAN_POINT('Ctrl Pts',(1.10000992106221,-1.29450057597768,0.692169783635984));
#10250=CARTESIAN_POINT('Ctrl Pts',(1.10000876843985,-1.28709422081189,0.695229417764685));
#10251=CARTESIAN_POINT('Ctrl Pts',(1.100005676647,-1.27938091857402,0.69743146309387));
#10252=CARTESIAN_POINT('Ctrl Pts',(1.10000309801581,-1.2715114871423,0.698709794160748));
#10253=CARTESIAN_POINT('Ctrl Pts',(1.10000138449209,-1.26628217885177,0.699559256705032));
#10254=CARTESIAN_POINT('Ctrl Pts',(1.1,-1.26098326598685,0.700000000000001));
#10255=CARTESIAN_POINT('Ctrl Pts',(1.1,-1.25565664448621,0.7));
#10256=CARTESIAN_POINT('',(1.1,-1.39262953588351,0.));
#10257=CARTESIAN_POINT('Ctrl Pts',(1.1,-1.39262953588351,0.));
#10258=CARTESIAN_POINT('Ctrl Pts',(1.1,-1.38665944902278,0.100890429980357));
#10259=CARTESIAN_POINT('Ctrl Pts',(1.1,-1.38068638286488,0.201781712214768));
#10260=CARTESIAN_POINT('Ctrl Pts',(1.1,-1.36872453529477,0.403729561179669));
#10261=CARTESIAN_POINT('Ctrl Pts',(1.10000000000005,-1.3627356212621,0.504788200493074));
#10262=CARTESIAN_POINT('Ctrl Pts',(1.10000000000005,-1.35674377243284,0.605845626926786));
#10263=CARTESIAN_POINT('',(1.1,-1.44962962962963,0.));
#10264=CARTESIAN_POINT('Origin',(0.199725906950915,-1.4,-0.0104671912485888));
#10265=CARTESIAN_POINT('',(0.200274469199584,1.15262458915154,1.38777878078145E-17));
#10266=CARTESIAN_POINT('',(0.200274469199585,-0.7,0.));
#10267=CARTESIAN_POINT('',(0.231993417893744,1.12115139781563,0.605233595624295));
#10268=CARTESIAN_POINT('Ctrl Pts',(0.200274469199584,1.15262458915154,-5.50774703622636E-17));
#10269=CARTESIAN_POINT('Ctrl Pts',(0.210847451072758,1.1421331482829,0.201744512318911));
#10270=CARTESIAN_POINT('Ctrl Pts',(0.221420433966108,1.13164208276446,0.403489044103923));
#10271=CARTESIAN_POINT('Ctrl Pts',(0.231993417893744,1.12115139781563,0.605233595624295));
#10272=CARTESIAN_POINT('',(0.231993417893744,-1.12115139781563,0.605233595624295));
#10273=CARTESIAN_POINT('',(0.231993417893744,-0.7,0.605233595624295));
#10274=CARTESIAN_POINT('',(0.200274469199584,-1.15262458915154,1.38777878078145E-17));
#10275=CARTESIAN_POINT('Ctrl Pts',(0.231993417893744,-1.12115139781563,
0.605233595624295));
#10276=CARTESIAN_POINT('Ctrl Pts',(0.221420433966108,-1.13164208276446,
0.403489044103923));
#10277=CARTESIAN_POINT('Ctrl Pts',(0.210847451072758,-1.1421331482829,0.201744512318911));
#10278=CARTESIAN_POINT('Ctrl Pts',(0.200274469199584,-1.15262458915154,
-6.67868538251071E-17));
#10279=CARTESIAN_POINT('',(0.200274469199585,-0.7,0.));
#10280=CARTESIAN_POINT('Origin',(6.07974599480623,0.,0.));
#10281=CARTESIAN_POINT('Ctrl Pts',(8.1,-1.69866351109718,4.37041895728907E-16));
#10282=CARTESIAN_POINT('Ctrl Pts',(8.9524267631348,-1.65897367198627,1.20944032620455E-7));
#10283=CARTESIAN_POINT('Ctrl Pts',(9.80407798130771,-1.59837060538327,2.76830114922109E-8));
#10284=CARTESIAN_POINT('Ctrl Pts',(10.6537697771985,-1.52488560579501,1.03413542584124E-8));
#10285=CARTESIAN_POINT('Ctrl Pts',(10.8359404901627,-1.50913069933138,6.62336842220622E-9));
#10286=CARTESIAN_POINT('Ctrl Pts',(11.0180211259896,-1.49278349820154,3.93228299510406E-9));
#10287=CARTESIAN_POINT('Ctrl Pts',(11.2000000002909,-1.47592264092474,-3.0227174540096E-11));
#10288=CARTESIAN_POINT('Ctrl Pts',(11.2000000002909,1.47592264092474,-3.02272213335841E-11));
#10289=CARTESIAN_POINT('Ctrl Pts',(10.4240589919717,1.54781576943643,1.68591524001238E-8));
#10290=CARTESIAN_POINT('Ctrl Pts',(9.64626799696257,1.61037563220813,6.17878738288937E-8));
#10291=CARTESIAN_POINT('Ctrl Pts',(8.86753211358286,1.65747704847969,5.27022751808308E-8));
#10292=CARTESIAN_POINT('Ctrl Pts',(8.61177933690776,1.67294611604661,4.97183789310355E-8));
#10293=CARTESIAN_POINT('Ctrl Pts',(8.35592462822135,1.68674740550612,3.63007687033005E-8));
#10294=CARTESIAN_POINT('Ctrl Pts',(8.1,1.69866351109718,3.71000138306103E-16));
#10295=CARTESIAN_POINT('',(7.9,1.70758761671949,0.));
#10296=CARTESIAN_POINT('',(7.9,1.7737037037037,0.));
#10297=CARTESIAN_POINT('Ctrl Pts',(7.90000000036908,1.70758761645525,-3.06814577203155E-11));
#10298=CARTESIAN_POINT('Ctrl Pts',(7.26247716501442,1.73478515342832,3.65175246633048E-8));
#10299=CARTESIAN_POINT('Ctrl Pts',(6.624575449312,1.74993328406844,-3.04558542439636E-7));
#10300=CARTESIAN_POINT('Ctrl Pts',(5.98677261990733,1.74972113442148,-3.1918790057331E-7));
#10301=CARTESIAN_POINT('Ctrl Pts',(5.35540610719671,1.74951112565922,-3.33669628155763E-7));
#10302=CARTESIAN_POINT('Ctrl Pts',(4.72663057529054,1.73425216511322,1.21151810208783E-7));
#10303=CARTESIAN_POINT('Ctrl Pts',(4.10000000045307,1.7011388979176,-4.27317258673188E-11));
#10304=CARTESIAN_POINT('',(3.9,1.68995649764597,0.));
#10305=CARTESIAN_POINT('',(3.9,1.7662962962963,0.));
#10306=CARTESIAN_POINT('Ctrl Pts',(3.9,1.68995649764597,-1.6113354923472E-17));
#10307=CARTESIAN_POINT('Ctrl Pts',(2.96252047830716,1.63464572816558,-1.61179993858831E-17));
#10308=CARTESIAN_POINT('Ctrl Pts',(2.02971500398675,1.53866944530133,-1.61823222708931E-17));
#10309=CARTESIAN_POINT('Ctrl Pts',(1.1,1.39262953588351,-1.60717230190728E-17));
#10310=CARTESIAN_POINT('',(0.9,1.3604297237941,0.));
#10311=CARTESIAN_POINT('',(0.9,1.44962962962963,0.));
#10312=CARTESIAN_POINT('',(0.28146619846596,1.25073018526678,0.));
#10313=CARTESIAN_POINT('Ctrl Pts',(0.899999999999963,1.36042972379409,2.53412200078296E-14));
#10314=CARTESIAN_POINT('Ctrl Pts',(0.693681964344164,1.32640030945436,-1.68820282978727E-7));
#10315=CARTESIAN_POINT('Ctrl Pts',(0.487510176034459,1.28986876146525,1.95094241611213E-11));
#10316=CARTESIAN_POINT('Ctrl Pts',(0.281466198465954,1.25073018526678,9.09211941846344E-16));
#10317=CARTESIAN_POINT('Ctrl Pts',(0.28146619846596,1.25073018526678,4.90059381963448E-17));
#10318=CARTESIAN_POINT('Ctrl Pts',(0.273672142824666,1.24924968434803,-1.60851827685828E-11));
#10319=CARTESIAN_POINT('Ctrl Pts',(0.266112037439191,1.2468180315926,-2.29735811958388E-6));
#10320=CARTESIAN_POINT('Ctrl Pts',(0.258922416881026,1.24354471831116,-3.39045428380668E-6));
#10321=CARTESIAN_POINT('Ctrl Pts',(0.254316658841251,1.24144779416325,-4.09070493067818E-6));
#10322=CARTESIAN_POINT('Ctrl Pts',(0.249862973385875,1.23900427835211,-4.3601744978078E-6));
#10323=CARTESIAN_POINT('Ctrl Pts',(0.245601965247185,1.23623285256398,-4.0505643599354E-6));
#10324=CARTESIAN_POINT('Ctrl Pts',(0.238945660500109,1.23190348870705,-3.5669089987193E-6));
#10325=CARTESIAN_POINT('Ctrl Pts',(0.232836306411817,1.22682685988243,-1.47564048465526E-6));
#10326=CARTESIAN_POINT('Ctrl Pts',(0.227416445112993,1.2210931256102,-3.43092614100725E-7));
#10327=CARTESIAN_POINT('Ctrl Pts',(0.225957664245637,1.21954986437275,-3.82620891408318E-8));
#10328=CARTESIAN_POINT('Ctrl Pts',(0.224549002474426,1.21795876469157,1.76022586487844E-7));
#10329=CARTESIAN_POINT('Ctrl Pts',(0.223193686986583,1.21632111005909,2.01577349231486E-7));
#10330=CARTESIAN_POINT('Ctrl Pts',(0.221344954485829,1.21408724984631,2.36435595047204E-7));
#10331=CARTESIAN_POINT('Ctrl Pts',(0.219595448227346,1.21176677459781,-7.7718209010198E-8));
#10332=CARTESIAN_POINT('Ctrl Pts',(0.217948412504407,1.20936721934621,-5.08402878561E-7));
#10333=CARTESIAN_POINT('Ctrl Pts',(0.213467776427723,1.20283941082417,-1.68004793834142E-6));
#10334=CARTESIAN_POINT('Ctrl Pts',(0.20978887558685,1.19579640990262,-3.43350901357988E-6));
#10335=CARTESIAN_POINT('Ctrl Pts',(0.206958221875648,1.18840352636746,-3.67425174897535E-6));
#10336=CARTESIAN_POINT('Ctrl Pts',(0.206193447398199,1.18640614723908,-3.7392946395744E-6));
#10337=CARTESIAN_POINT('Ctrl Pts',(0.205490847532167,1.18438308363371,-3.7149036306613E-6));
#10338=CARTESIAN_POINT('Ctrl Pts',(0.204851940804359,1.18233735619935,-3.6037364623937E-6));
#10339=CARTESIAN_POINT('Ctrl Pts',(0.202492508448082,1.17478264548698,-3.19320484275276E-6));
#10340=CARTESIAN_POINT('Ctrl Pts',(0.201019195184615,1.16698811697394,-1.36638523817118E-6));
#10341=CARTESIAN_POINT('Ctrl Pts',(0.200491965466086,1.15911075533121,-4.28455138775697E-7));
#10342=CARTESIAN_POINT('Ctrl Pts',(0.200347608840846,1.15695391685535,-1.71647870329038E-7));
#10343=CARTESIAN_POINT('Ctrl Pts',(0.200274469313241,1.15479080601565,-7.49035961899928E-12));
#10344=CARTESIAN_POINT('Ctrl Pts',(0.200274469199584,1.15262458915154,9.10729824887824E-18));
#10345=CARTESIAN_POINT('',(2.01407162049393E-18,1.15316892111334,2.77409355997279E-17));
#10346=CARTESIAN_POINT('',(0.,-1.4,0.));
#10347=CARTESIAN_POINT('',(0.243580684154574,1.44748675362873,2.77555756156289E-17));
#10348=CARTESIAN_POINT('Ctrl Pts',(0.243580684154575,1.44748675362873,-1.56125112837913E-16));
#10349=CARTESIAN_POINT('Ctrl Pts',(0.226022619058538,1.44415189332774,-6.74769223000006E-12));
#10350=CARTESIAN_POINT('Ctrl Pts',(0.208837776424359,1.43922483814223,-1.83343972289099E-6));
#10351=CARTESIAN_POINT('Ctrl Pts',(0.192216855517481,1.43283671850359,-2.37047811876899E-6));
#10352=CARTESIAN_POINT('Ctrl Pts',(0.175448307189507,1.42639185943196,-2.91228650265529E-6));
#10353=CARTESIAN_POINT('Ctrl Pts',(0.15925228528901,1.41845922211561,-2.09168970691363E-6));
#10354=CARTESIAN_POINT('Ctrl Pts',(0.143842215871583,1.4091253227419,-1.20497646612983E-7));
#10355=CARTESIAN_POINT('Ctrl Pts',(0.141154971457358,1.40749765525544,2.23243494969264E-7));
#10356=CARTESIAN_POINT('Ctrl Pts',(0.138491701959641,1.40582727297256,5.92673833856784E-7));
#10357=CARTESIAN_POINT('Ctrl Pts',(0.135853645420207,1.40411450883245,9.74556207071009E-7));
#10358=CARTESIAN_POINT('Ctrl Pts',(0.120686164410185,1.39426698768136,3.17018528370531E-6));
#10359=CARTESIAN_POINT('Ctrl Pts',(0.106484701177391,1.38310949089167,6.09567884445769E-6));
#10360=CARTESIAN_POINT('Ctrl Pts',(0.0934509959242968,1.37075049507673,
5.10227143121889E-6));
#10361=CARTESIAN_POINT('Ctrl Pts',(0.0918301157095608,1.36921352217444,
4.97873062758527E-6));
#10362=CARTESIAN_POINT('Ctrl Pts',(0.0902273306836925,1.36765791150105,
4.78983320752683E-6));
#10363=CARTESIAN_POINT('Ctrl Pts',(0.0886430622088043,1.36608382581751,
4.52250464763623E-6));
#10364=CARTESIAN_POINT('Ctrl Pts',(0.0755027622673366,1.35302798437193,
2.30521792157715E-6));
#10365=CARTESIAN_POINT('Ctrl Pts',(0.0636322991078783,1.33870385142449,
-4.95851449924696E-6));
#10366=CARTESIAN_POINT('Ctrl Pts',(0.0531272107863483,1.3233265665666,-1.07771754856876E-5));
#10367=CARTESIAN_POINT('Ctrl Pts',(0.0429100363670196,1.3083707283404,-1.64363639061758E-5));
#10368=CARTESIAN_POINT('Ctrl Pts',(0.0340657397255946,1.29253754778979,
-2.07072841115287E-5));
#10369=CARTESIAN_POINT('Ctrl Pts',(0.026663056477648,1.27603964904139,-2.15377272154938E-5));
#10370=CARTESIAN_POINT('Ctrl Pts',(0.0217318501145713,1.26504977678014,
-2.20909166714363E-5));
#10371=CARTESIAN_POINT('Ctrl Pts',(0.0174411483101006,1.25376411673155,
-2.12025196266096E-5));
#10372=CARTESIAN_POINT('Ctrl Pts',(0.01382286588119,1.24224013948332,-1.91534441809703E-5));
#10373=CARTESIAN_POINT('Ctrl Pts',(0.00842668188255806,1.22505366970124,
-1.60975223868617E-5));
#10374=CARTESIAN_POINT('Ctrl Pts',(0.00456091079961661,1.20745571355567,
-1.03588883906395E-5));
#10375=CARTESIAN_POINT('Ctrl Pts',(0.0023097402764219,1.18964331095195,
-5.71664032024866E-6));
#10376=CARTESIAN_POINT('Ctrl Pts',(0.00078319128522165,1.17756448131848,
-2.56866950429304E-6));
#10377=CARTESIAN_POINT('Ctrl Pts',(2.50028438421117E-9,1.16538650529032,
-1.91718613723104E-10));
#10378=CARTESIAN_POINT('Ctrl Pts',(-1.21430643318376E-17,1.15316892111333,
5.20417042793042E-18));
#10379=CARTESIAN_POINT('',(11.7295909468525,1.62672708026858,5.55111512312578E-17));
#10380=CARTESIAN_POINT('Ctrl Pts',(0.243580684154574,1.44748675362873,0.));
#10381=CARTESIAN_POINT('Ctrl Pts',(4.07225077172054,2.17467835246083,0.));
#10382=CARTESIAN_POINT('Ctrl Pts',(7.90092085928651,2.00057770191527,0.));
#10383=CARTESIAN_POINT('Ctrl Pts',(11.7295909468525,1.62672708026858,0.));
#10384=CARTESIAN_POINT('',(12.,1.32855945177638,-4.17473993839455E-17));
#10385=CARTESIAN_POINT('Ctrl Pts',(12.,1.32855945177638,2.42861286636753E-16));
#10386=CARTESIAN_POINT('Ctrl Pts',(11.9999999991614,1.34640852075174,-1.28298622986823E-11));
#10387=CARTESIAN_POINT('Ctrl Pts',(11.9983618543561,1.36418409382152,-2.22383001277967E-6));
#10388=CARTESIAN_POINT('Ctrl Pts',(11.9951861391139,1.38167870884165,-3.43465861540838E-6));
#10389=CARTESIAN_POINT('Ctrl Pts',(11.9919727904737,1.39938064150867,-4.65983598400874E-6));
#10390=CARTESIAN_POINT('Ctrl Pts',(11.9871848331028,1.41679645887758,-4.78742071954366E-6));
#10391=CARTESIAN_POINT('Ctrl Pts',(11.9808755917115,1.43370272794343,-3.5739118077222E-6));
#10392=CARTESIAN_POINT('Ctrl Pts',(11.9797611226834,1.43668906371449,-3.35955670324834E-6));
#10393=CARTESIAN_POINT('Ctrl Pts',(11.9785990681726,1.43965944485564,-3.11247275469786E-6));
#10394=CARTESIAN_POINT('Ctrl Pts',(11.9773895732386,1.44261255525912,-2.84353511336506E-6));
#10395=CARTESIAN_POINT('Ctrl Pts',(11.9705369081732,1.45934406518776,-1.31980853313606E-6));
#10396=CARTESIAN_POINT('Ctrl Pts',(11.9622259501015,1.47537448669426,1.24030492427686E-6));
#10397=CARTESIAN_POINT('Ctrl Pts',(11.9525330320198,1.49048867890869,8.79804099270529E-7));
#10398=CARTESIAN_POINT('Ctrl Pts',(11.9492586078121,1.49559449703792,7.58021100761347E-7));
#10399=CARTESIAN_POINT('Ctrl Pts',(11.9458260650319,1.50059560584699,2.73671093112169E-7));
#10400=CARTESIAN_POINT('Ctrl Pts',(11.9422371454499,1.50548309160802,-8.21070286398525E-7));
#10401=CARTESIAN_POINT('Ctrl Pts',(11.9335276940755,1.51734385321214,-3.47774636801117E-6));
#10402=CARTESIAN_POINT('Ctrl Pts',(11.923898315087,1.52853671512454,-9.61160164537397E-6));
#10403=CARTESIAN_POINT('Ctrl Pts',(11.9134480753511,1.53899918600446,-1.54908303532852E-5));
#10404=CARTESIAN_POINT('Ctrl Pts',(11.9006414429521,1.55182080751067,-2.26957483986032E-5));
#10405=CARTESIAN_POINT('Ctrl Pts',(11.8867118754531,1.56343792791748,-2.93307907620841E-5));
#10406=CARTESIAN_POINT('Ctrl Pts',(11.8718669715436,1.57375979462261,-3.2097080434168E-5));
#10407=CARTESIAN_POINT('Ctrl Pts',(11.8583226919989,1.58317731924447,-3.46210038525051E-5));
#10408=CARTESIAN_POINT('Ctrl Pts',(11.84401509256,1.59151672629289,-3.39892197405707E-5));
#10409=CARTESIAN_POINT('Ctrl Pts',(11.8290799708805,1.59867837245092,-3.04453078860132E-5));
#10410=CARTESIAN_POINT('Ctrl Pts',(11.8128282236205,1.60647136308226,-2.65889777530425E-5));
#10411=CARTESIAN_POINT('Ctrl Pts',(11.7959622791259,1.61280865470064,-1.93051308245346E-5));
#10412=CARTESIAN_POINT('Ctrl Pts',(11.7786680578171,1.61758555622507,-1.24065785496921E-5));
#10413=CARTESIAN_POINT('Ctrl Pts',(11.7626326571209,1.62201475420184,-6.0101616208217E-6));
#10414=CARTESIAN_POINT('Ctrl Pts',(11.7462278952123,1.62510256303752,-1.15598952599692E-10));
#10415=CARTESIAN_POINT('Ctrl Pts',(11.7295909468525,1.62672708026857,-1.01481323344643E-16));
#10416=CARTESIAN_POINT('',(12.,-1.32855945177638,-2.7831599589297E-17));
#10417=CARTESIAN_POINT('',(12.,1.6,0.));
#10418=CARTESIAN_POINT('',(11.7295909468525,-1.62672708026858,-2.77555756156289E-17));
#10419=CARTESIAN_POINT('Ctrl Pts',(11.7295909468525,-1.62672708026858,2.76688394418301E-16));
#10420=CARTESIAN_POINT('Ctrl Pts',(11.7473502233519,-1.62499297457843,3.63491969896433E-13));
#10421=CARTESIAN_POINT('Ctrl Pts',(11.7648769397846,-1.62163540491215,-2.46542030701863E-6));
#10422=CARTESIAN_POINT('Ctrl Pts',(11.7819744899096,-1.61677476461769,-3.87870576098494E-6));
#10423=CARTESIAN_POINT('Ctrl Pts',(11.799277951102,-1.61185558613358,-5.30901184740094E-6));
#10424=CARTESIAN_POINT('Ctrl Pts',(11.8161433440738,-1.60539638769883,-5.61072687595782E-6));
#10425=CARTESIAN_POINT('Ctrl Pts',(11.8323535184498,-1.59747214364331,-4.43708131311936E-6));
#10426=CARTESIAN_POINT('Ctrl Pts',(11.8351986841263,-1.59608130189932,-4.23108623901291E-6));
#10427=CARTESIAN_POINT('Ctrl Pts',(11.8380235988884,-1.59464521634493,-3.98890160078043E-6));
#10428=CARTESIAN_POINT('Ctrl Pts',(11.8408269920241,-1.59316415515964,-3.72087260345577E-6));
#10429=CARTESIAN_POINT('Ctrl Pts',(11.8568148563263,-1.58471760338924,-2.19229240409177E-6));
#10430=CARTESIAN_POINT('Ctrl Pts',(11.8719627312575,-1.57488689795395,5.08047814114288E-7));
#10431=CARTESIAN_POINT('Ctrl Pts',(11.8860639991294,-1.56376935451958,3.7910357452838E-7));
#10432=CARTESIAN_POINT('Ctrl Pts',(11.8908390360804,-1.5600046802233,3.35439876042474E-7));
#10433=CARTESIAN_POINT('Ctrl Pts',(11.8954938739134,-1.55609205312677,-6.31409548673105E-8));
#10434=CARTESIAN_POINT('Ctrl Pts',(11.9000197537765,-1.55203410647271,-1.07033715310124E-6));
#10435=CARTESIAN_POINT('Ctrl Pts',(11.9109521284419,-1.54223203603875,-3.50324446252274E-6));
#10436=CARTESIAN_POINT('Ctrl Pts',(11.9211333865357,-1.53158293117673,-9.37257606292525E-6));
#10437=CARTESIAN_POINT('Ctrl Pts',(11.9305114837192,-1.52019095639426,-1.50133174764804E-5));
#10438=CARTESIAN_POINT('Ctrl Pts',(11.9420285825687,-1.50620064502377,-2.19406264148308E-5));
#10439=CARTESIAN_POINT('Ctrl Pts',(11.9522379825693,-1.49120969914507,-2.8349487615449E-5));
#10440=CARTESIAN_POINT('Ctrl Pts',(11.9610699533786,-1.47543375940277,-3.10096306454085E-5));
#10441=CARTESIAN_POINT('Ctrl Pts',(11.9691383866925,-1.46102167397773,-3.34398002084833E-5));
#10442=CARTESIAN_POINT('Ctrl Pts',(11.976057247492,-1.44595309822982,-3.28127654573608E-5));
#10443=CARTESIAN_POINT('Ctrl Pts',(11.9817405815488,-1.43037347552767,-2.93737351251587E-5));
#10444=CARTESIAN_POINT('Ctrl Pts',(11.9879190063177,-1.41343666945002,-2.56351214921306E-5));
#10445=CARTESIAN_POINT('Ctrl Pts',(11.9925890154887,-1.39602986621001,-1.86015881889918E-5));
#10446=CARTESIAN_POINT('Ctrl Pts',(11.9956646601292,-1.37834843064327,-1.1951505214167E-5));
#10447=CARTESIAN_POINT('Ctrl Pts',(11.9985188379205,-1.36194017591583,-5.78027239782095E-6));
#10448=CARTESIAN_POINT('Ctrl Pts',(11.9999999979315,-1.34529424449622,-1.63143103698095E-10));
#10449=CARTESIAN_POINT('Ctrl Pts',(12.,-1.32855945177638,6.07153216591882E-17));
#10450=CARTESIAN_POINT('',(0.243580684154574,-1.44748675362873,-2.77555756156289E-17));
#10451=CARTESIAN_POINT('Ctrl Pts',(11.7295909468525,-1.62672708026858,0.));
#10452=CARTESIAN_POINT('Ctrl Pts',(7.90092085928651,-2.00057770191527,0.));
#10453=CARTESIAN_POINT('Ctrl Pts',(4.07225077172054,-2.17467835246083,0.));
#10454=CARTESIAN_POINT('Ctrl Pts',(0.243580684154574,-1.44748675362873,
0.));
#10455=CARTESIAN_POINT('',(-2.01407162049393E-18,-1.15316892111334,-2.77409355997279E-17));
#10456=CARTESIAN_POINT('Ctrl Pts',(-1.45716771982052E-16,-1.15316892111333,
-8.67361737988404E-17));
#10457=CARTESIAN_POINT('Ctrl Pts',(1.25998894435939E-9,-1.17105087373522,
-1.90287520688926E-11));
#10458=CARTESIAN_POINT('Ctrl Pts',(0.00163339464743996,-1.18886359576077,
-1.42965894531121E-6));
#10459=CARTESIAN_POINT('Ctrl Pts',(0.00480727841906161,-1.20639511031145,
-1.64093682142839E-6));
#10460=CARTESIAN_POINT('Ctrl Pts',(0.00800796397580062,-1.22407466931478,
-1.8539988284852E-6));
#10461=CARTESIAN_POINT('Ctrl Pts',(0.0127756311263789,-1.24146980201313,
-7.66483898132055E-7));
#10462=CARTESIAN_POINT('Ctrl Pts',(0.0190655400899108,-1.25835467436912,
1.24978183846727E-6));
#10463=CARTESIAN_POINT('Ctrl Pts',(0.0201762582672253,-1.26133632875492,
1.60582880463507E-6));
#10464=CARTESIAN_POINT('Ctrl Pts',(0.0213345630164365,-1.2643020159517,
1.98173645466097E-6));
#10465=CARTESIAN_POINT('Ctrl Pts',(0.022540357064946,-1.26725040777374,
2.36324320385681E-6));
#10466=CARTESIAN_POINT('Ctrl Pts',(0.0293845669280623,-1.28398578013164,
4.5287143794027E-6));
#10467=CARTESIAN_POINT('Ctrl Pts',(0.0376942987862453,-1.30001720705818,
7.20349268724091E-6));
#10468=CARTESIAN_POINT('Ctrl Pts',(0.0474014865253391,-1.31512615530125,
5.82569015349308E-6));
#10469=CARTESIAN_POINT('Ctrl Pts',(0.0485928463173857,-1.31698047129067,
5.65659292531477E-6));
#10470=CARTESIAN_POINT('Ctrl Pts',(0.049805315173965,-1.3188208685659,5.4220814195758E-6));
#10471=CARTESIAN_POINT('Ctrl Pts',(0.0510388164126442,-1.32064691964073,
5.10992468070797E-6));
#10472=CARTESIAN_POINT('Ctrl Pts',(0.0614399911345998,-1.33604461498541,
2.47774509321499E-6));
#10473=CARTESIAN_POINT('Ctrl Pts',(0.0733332132114129,-1.35042574344132,
-5.3152380038924E-6));
#10474=CARTESIAN_POINT('Ctrl Pts',(0.0865238753361435,-1.36365441213776,
-1.1550981620978E-5));
#10475=CARTESIAN_POINT('Ctrl Pts',(0.0993129767592984,-1.37648036310613,
-1.75968917362996E-5));
#10476=CARTESIAN_POINT('Ctrl Pts',(0.113220041589059,-1.38812080263946,
-2.21381304374214E-5));
#10477=CARTESIAN_POINT('Ctrl Pts',(0.128049501721596,-1.3984678073416,-2.30260298918279E-5));
#10478=CARTESIAN_POINT('Ctrl Pts',(0.137898881094142,-1.40534004502052,
-2.36157518704412E-5));
#10479=CARTESIAN_POINT('Ctrl Pts',(0.148156110210342,-1.41164106947418,
-2.26770903305374E-5));
#10480=CARTESIAN_POINT('Ctrl Pts',(0.158771208267938,-1.41732893485082,
-2.05010084084185E-5));
#10481=CARTESIAN_POINT('Ctrl Pts',(0.174640735071984,-1.42583226958806,
-1.72477751171679E-5));
#10482=CARTESIAN_POINT('Ctrl Pts',(0.191199787345415,-1.4329086754137,-1.11085100333009E-5));
#10483=CARTESIAN_POINT('Ctrl Pts',(0.208270835533445,-1.43843835369108,
-6.12965879291162E-6));
#10484=CARTESIAN_POINT('Ctrl Pts',(0.219822542278978,-1.44218019901621,
-2.76054936125183E-6));
#10485=CARTESIAN_POINT('Ctrl Pts',(0.231609382520684,-1.4452130041726,-1.10646384277296E-10));
#10486=CARTESIAN_POINT('Ctrl Pts',(0.243580684154575,-1.44748675362873,
-8.67361737988404E-18));
#10487=CARTESIAN_POINT('',(0.,-1.4,0.));
#10488=CARTESIAN_POINT('',(0.28146619846596,-1.25073018526678,-1.38777878078145E-17));
#10489=CARTESIAN_POINT('Ctrl Pts',(0.200274469199584,-1.15262458915154,
-4.38017677684144E-17));
#10490=CARTESIAN_POINT('Ctrl Pts',(0.200274469606231,-1.16056122076396,
-2.67994619525583E-11));
#10491=CARTESIAN_POINT('Ctrl Pts',(0.201251993787099,-1.16844573575355,
-2.06906772440415E-6));
#10492=CARTESIAN_POINT('Ctrl Pts',(0.203125250303271,-1.17612349127761,
-3.03593176598444E-6));
#10493=CARTESIAN_POINT('Ctrl Pts',(0.204328175564463,-1.18105381768481,
-3.65681052429326E-6));
#10494=CARTESIAN_POINT('Ctrl Pts',(0.205901645655995,-1.18589907428975,
-3.87486521964464E-6));
#10495=CARTESIAN_POINT('Ctrl Pts',(0.207834893326199,-1.19061551412018,
-3.56660141708203E-6));
#10496=CARTESIAN_POINT('Ctrl Pts',(0.210845733886816,-1.19796089907112,
-3.08651126907409E-6));
#10497=CARTESIAN_POINT('Ctrl Pts',(0.214691665920849,-1.20490884791767,
-1.13290501265697E-6));
#10498=CARTESIAN_POINT('Ctrl Pts',(0.219311372289421,-1.21130241743461,
-1.88024479619773E-7));
#10499=CARTESIAN_POINT('Ctrl Pts',(0.220549822002528,-1.21301640393121,
6.52788543367939E-8));
#10500=CARTESIAN_POINT('Ctrl Pts',(0.22184414018537,-1.21469042595737,2.26073670777299E-7));
#10501=CARTESIAN_POINT('Ctrl Pts',(0.223193686901845,-1.21632111014354,
1.99977909429435E-7));
#10502=CARTESIAN_POINT('Ctrl Pts',(0.225054776233359,-1.21856990146355,
1.63990609064731E-7));
#10503=CARTESIAN_POINT('Ctrl Pts',(0.227020882846909,-1.2207363067163,-2.2494482424301E-7));
#10504=CARTESIAN_POINT('Ctrl Pts',(0.229085096241527,-1.22281561536867,
-7.25033596408456E-7));
#10505=CARTESIAN_POINT('Ctrl Pts',(0.234663732853057,-1.22843504764494,
-2.07654770860772E-6));
#10506=CARTESIAN_POINT('Ctrl Pts',(0.240898147116973,-1.23336261820331,
-3.93931381885212E-6));
#10507=CARTESIAN_POINT('Ctrl Pts',(0.247634917667946,-1.2375211924479,-4.15647360184107E-6));
#10508=CARTESIAN_POINT('Ctrl Pts',(0.24944409362824,-1.23863798757926,-4.21479238469909E-6));
#10509=CARTESIAN_POINT('Ctrl Pts',(0.251289686356224,-1.23969909864123,
-4.17584617698396E-6));
#10510=CARTESIAN_POINT('Ctrl Pts',(0.253169062337335,-1.24070249413235,
-4.04352721072409E-6));
#10511=CARTESIAN_POINT('Ctrl Pts',(0.260147540238377,-1.24442829106235,
-3.55220190316667E-6));
#10512=CARTESIAN_POINT('Ctrl Pts',(0.267526846148503,-1.24732811138375,
-1.51439637010182E-6));
#10513=CARTESIAN_POINT('Ctrl Pts',(0.275164162321015,-1.24931347733136,
-4.73394739174148E-7));
#10514=CARTESIAN_POINT('Ctrl Pts',(0.277246452424842,-1.24985478107889,
-1.89568936341825E-7));
#10515=CARTESIAN_POINT('Ctrl Pts',(0.27934803608603,-1.25032783487679,-4.20368826828312E-12));
#10516=CARTESIAN_POINT('Ctrl Pts',(0.28146619846596,-1.25073018526678,1.2793585635329E-17));
#10517=CARTESIAN_POINT('',(0.9,-1.3604297237941,0.));
#10518=CARTESIAN_POINT('Ctrl Pts',(0.281466198465954,-1.25073018526678,
9.63150999927498E-16));
#10519=CARTESIAN_POINT('Ctrl Pts',(0.487510152792939,-1.28986875705046,
1.95065110193295E-11));
#10520=CARTESIAN_POINT('Ctrl Pts',(0.693681940810289,-1.32640030557063,
-1.68784634270162E-7));
#10521=CARTESIAN_POINT('Ctrl Pts',(0.899999999999961,-1.36042972379409,
2.52314774976951E-14));
#10522=CARTESIAN_POINT('',(0.9,1.44962962962963,0.));
#10523=CARTESIAN_POINT('',(3.9,-1.68995649764597,0.));
#10524=CARTESIAN_POINT('Ctrl Pts',(1.1,-1.39262953588351,-2.05019623674552E-17));
#10525=CARTESIAN_POINT('Ctrl Pts',(2.02971449277185,-1.53866936499954,-2.04062575199768E-17));
#10526=CARTESIAN_POINT('Ctrl Pts',(2.96251993741879,-1.63464569625347,-2.05230086706555E-17));
#10527=CARTESIAN_POINT('Ctrl Pts',(3.9,-1.68995649764597,-2.05203881127908E-17));
#10528=CARTESIAN_POINT('',(3.9,1.7662962962963,0.));
#10529=CARTESIAN_POINT('',(7.9,-1.70758761671949,0.));
#10530=CARTESIAN_POINT('Ctrl Pts',(4.10000000045307,-1.7011388979176,-4.27317380631109E-11));
#10531=CARTESIAN_POINT('Ctrl Pts',(4.72643887491804,-1.7342420350347,1.20853286712337E-7));
#10532=CARTESIAN_POINT('Ctrl Pts',(5.35502164560988,-1.74950180199062,-3.33551248611792E-7));
#10533=CARTESIAN_POINT('Ctrl Pts',(5.98619394951577,-1.74972093772735,-3.1920111515717E-7));
#10534=CARTESIAN_POINT('Ctrl Pts',(6.62418968669829,-1.74994244248134,-3.0469584628258E-7));
#10535=CARTESIAN_POINT('Ctrl Pts',(7.26228442347589,-1.73479337602516,3.6583895104054E-8));
#10536=CARTESIAN_POINT('Ctrl Pts',(7.90000000036908,-1.70758761645525,-3.06816097140251E-11));
#10537=CARTESIAN_POINT('',(7.9,1.7737037037037,0.));
#10538=CARTESIAN_POINT('',(11.4,-1.45718524058191,0.));
#10539=CARTESIAN_POINT('',(11.7095901160181,-1.42740242188993,1.38777878078145E-17));
#10540=CARTESIAN_POINT('Ctrl Pts',(11.4000000008084,-1.45718524050535,1.02728155843002E-16));
#10541=CARTESIAN_POINT('Ctrl Pts',(11.5032315878449,-1.44740895658952,-1.62414911853346E-10));
#10542=CARTESIAN_POINT('Ctrl Pts',(11.6064290066394,-1.43747657129068,3.17212713797596E-13));
#10543=CARTESIAN_POINT('Ctrl Pts',(11.7095901160181,-1.42740242188993,-1.31135713082882E-16));
#10544=CARTESIAN_POINT('',(11.7997255308004,-1.32801330383774,0.));
#10545=CARTESIAN_POINT('Ctrl Pts',(11.7095901160181,-1.42740242188993,-9.19403442267708E-17));
#10546=CARTESIAN_POINT('Ctrl Pts',(11.7174875668098,-1.42663119997609,-1.06723531187443E-12));
#10547=CARTESIAN_POINT('Ctrl Pts',(11.7252481284326,-1.42489860698852,-1.31351091787008E-6));
#10548=CARTESIAN_POINT('Ctrl Pts',(11.7327147629935,-1.4222933789697,-1.57347087725304E-6));
#10549=CARTESIAN_POINT('Ctrl Pts',(11.7375034508718,-1.42062252930751,-1.7401948673154E-6));
#10550=CARTESIAN_POINT('Ctrl Pts',(11.742171336984,-1.41859157258352,-1.52962160850981E-6));
#10551=CARTESIAN_POINT('Ctrl Pts',(11.7466731630754,-1.4162133745499,-1.06822103866601E-6));
#10552=CARTESIAN_POINT('Ctrl Pts',(11.7538080604269,-1.41244419322064,-3.36952074275293E-7));
#10553=CARTESIAN_POINT('Ctrl Pts',(11.7604421378066,-1.40785009750528,1.23525126371337E-6));
#10554=CARTESIAN_POINT('Ctrl Pts',(11.7664060685299,-1.40250292630552,-7.85770423176645E-8));
#10555=CARTESIAN_POINT('Ctrl Pts',(11.7700505374369,-1.39923534992309,-8.81437879006801E-7));
#10556=CARTESIAN_POINT('Ctrl Pts',(11.7734443324447,-1.39568546479044,-2.84121358692309E-6));
#10557=CARTESIAN_POINT('Ctrl Pts',(11.7765701913309,-1.39188797822873,-4.73246891796253E-6));
#10558=CARTESIAN_POINT('Ctrl Pts',(11.7816218974528,-1.38575085342217,-7.78893003218221E-6));
#10559=CARTESIAN_POINT('Ctrl Pts',(11.7859196635778,-1.3790373064984,-1.04294718165207E-5));
#10560=CARTESIAN_POINT('Ctrl Pts',(11.7894058487846,-1.37190723377291,-1.0649753115785E-5));
#10561=CARTESIAN_POINT('Ctrl Pts',(11.7909886780302,-1.36866997385604,-1.07497672177443E-5));
#10562=CARTESIAN_POINT('Ctrl Pts',(11.7924036476919,-1.36534638272796,-1.04045251440782E-5));
#10563=CARTESIAN_POINT('Ctrl Pts',(11.7936422141268,-1.36194984358789,-9.67400732978531E-6));
#10564=CARTESIAN_POINT('Ctrl Pts',(11.7963517531347,-1.35451943450186,-8.0758964348484E-6));
#10565=CARTESIAN_POINT('Ctrl Pts',(11.7981920551596,-1.34681816044402,-4.45435127417515E-6));
#10566=CARTESIAN_POINT('Ctrl Pts',(11.7990923524223,-1.33899256731255,-1.99131993767782E-6));
#10567=CARTESIAN_POINT('Ctrl Pts',(11.7995108157868,-1.33535518645399,-8.46488755312323E-7));
#10568=CARTESIAN_POINT('Ctrl Pts',(11.7997255306472,-1.33169069466208,-1.20180646731727E-11));
#10569=CARTESIAN_POINT('Ctrl Pts',(11.7997255308004,-1.32801330383774,1.56125112837913E-17));
#10570=CARTESIAN_POINT('',(11.7997255308004,1.32801330383774,-1.38777878078145E-17));
#10571=CARTESIAN_POINT('',(11.7997255308004,0.8,0.));
#10572=CARTESIAN_POINT('',(11.7095901160181,1.42740242188993,1.38777878078145E-17));
#10573=CARTESIAN_POINT('Ctrl Pts',(11.7997255308004,1.32801330383774,3.29597460435593E-17));
#10574=CARTESIAN_POINT('Ctrl Pts',(11.7997255306701,1.33594993357028,-3.19998942079111E-12));
#10575=CARTESIAN_POINT('Ctrl Pts',(11.7987557313351,1.34384388324515,-1.1738056914779E-6));
#10576=CARTESIAN_POINT('Ctrl Pts',(11.7968890528831,1.35153020534854,-1.35082478761126E-6));
#10577=CARTESIAN_POINT('Ctrl Pts',(11.7956902940742,1.35646627043222,-1.46450435604653E-6));
#10578=CARTESIAN_POINT('Ctrl Pts',(11.7941204989552,1.36131691981906,-1.21679535622301E-6));
#10579=CARTESIAN_POINT('Ctrl Pts',(11.7921880664813,1.36603565236267,-7.51718013047842E-7));
#10580=CARTESIAN_POINT('Ctrl Pts',(11.7891321441143,1.37349779167052,-1.62510435539431E-8));
#10581=CARTESIAN_POINT('Ctrl Pts',(11.7852081688769,1.38054242009704,1.47305143123643E-6));
#10582=CARTESIAN_POINT('Ctrl Pts',(11.7804707482717,1.38699431162271,4.31295153147674E-8));
#10583=CARTESIAN_POINT('Ctrl Pts',(11.7775673564694,1.39094843993989,-8.33217322910001E-7));
#10584=CARTESIAN_POINT('Ctrl Pts',(11.774357304366,1.39467961749964,-2.88177890715362E-6));
#10585=CARTESIAN_POINT('Ctrl Pts',(11.7708736118052,1.39816709864095,-4.85419454747415E-6));
#10586=CARTESIAN_POINT('Ctrl Pts',(11.7652557092992,1.40379111072049,-8.03496856102318E-6));
#10587=CARTESIAN_POINT('Ctrl Pts',(11.7589908599241,1.40872063947841,-1.07717451179728E-5));
#10588=CARTESIAN_POINT('Ctrl Pts',(11.7522324303862,1.41288246393566,-1.10093962897399E-5));
#10589=CARTESIAN_POINT('Ctrl Pts',(11.7491699691574,1.41476832010531,-1.11170836593312E-5));
#10590=CARTESIAN_POINT('Ctrl Pts',(11.7460056456443,1.41649603445901,-1.07652933077188E-5));
#10591=CARTESIAN_POINT('Ctrl Pts',(11.7427518690514,1.41805582819498,-1.00150721194158E-5));
#10592=CARTESIAN_POINT('Ctrl Pts',(11.7356218627913,1.421473806899,-8.37111113549047E-6));
#10593=CARTESIAN_POINT('Ctrl Pts',(11.7281378774234,1.42405291512428,-4.62166314666036E-6));
#10594=CARTESIAN_POINT('Ctrl Pts',(11.7204387731059,1.42570834923663,-2.06587013620581E-6));
#10595=CARTESIAN_POINT('Ctrl Pts',(11.7168648812537,1.42647679479109,-8.79481766934018E-7));
#10596=CARTESIAN_POINT('Ctrl Pts',(11.7132443218769,1.42704557200794,-8.45784208685192E-12));
#10597=CARTESIAN_POINT('Ctrl Pts',(11.7095901160181,1.42740242188993,2.53703308361608E-17));
#10598=CARTESIAN_POINT('',(11.4,1.45718524058191,0.));
#10599=CARTESIAN_POINT('Ctrl Pts',(11.7095901160181,1.42740242188993,-2.09644042577228E-16));
#10600=CARTESIAN_POINT('Ctrl Pts',(11.6064290073882,1.43747657121756,3.16925904777201E-13));
#10601=CARTESIAN_POINT('Ctrl Pts',(11.5032315885351,1.44740895652415,-1.62368751268212E-10));
#10602=CARTESIAN_POINT('Ctrl Pts',(11.4000000008083,1.45718524050537,-7.57963810214684E-17));
#10603=CARTESIAN_POINT('',(11.4,-1.53779953703704,0.));
#10604=CARTESIAN_POINT('Origin',(10.,0.,0.));
#10605=CARTESIAN_POINT('',(9.6,-4.89858719658942E-17,0.7));
#10606=CARTESIAN_POINT('Origin',(10.,0.,0.7));
#10607=CARTESIAN_POINT('',(9.6,-4.89858719658942E-17,0.));
#10608=CARTESIAN_POINT('Origin',(2.,0.,0.));
#10609=CARTESIAN_POINT('',(1.6,-4.89858719658941E-17,0.7));
#10610=CARTESIAN_POINT('Origin',(2.,0.,0.7));
#10611=CARTESIAN_POINT('',(1.6,-4.89858719658941E-17,0.));
#10612=CARTESIAN_POINT('Origin',(11.4,-1.53779953703704,0.));
#10613=CARTESIAN_POINT('',(11.4,-1.4227102204299,0.605660349289938));
#10614=CARTESIAN_POINT('Ctrl Pts',(11.4,-1.45718524058191,0.));
#10615=CARTESIAN_POINT('Ctrl Pts',(11.4,-1.45144762186897,0.100853500740053));
#10616=CARTESIAN_POINT('Ctrl Pts',(11.4,-1.44570843451869,0.201707502489292));
#10617=CARTESIAN_POINT('Ctrl Pts',(11.4,-1.43421679834229,0.403593890565801));
#10618=CARTESIAN_POINT('Ctrl Pts',(11.4,-1.42846427656079,0.504627461196798));
#10619=CARTESIAN_POINT('Ctrl Pts',(11.4,-1.4227102204299,0.605660349289938));
#10620=CARTESIAN_POINT('',(11.4,1.4227102204299,0.605660349289938));
#10621=CARTESIAN_POINT('Ctrl Pts',(11.4,1.4227102204299,0.605660349289938));
#10622=CARTESIAN_POINT('Ctrl Pts',(11.4,1.42846501637408,0.504614471147338));
#10623=CARTESIAN_POINT('Ctrl Pts',(11.4,1.43421827757761,0.403567910233218));
#10624=CARTESIAN_POINT('Ctrl Pts',(11.4,1.44570991295315,0.201681522149997));
#10625=CARTESIAN_POINT('Ctrl Pts',(11.4,1.45144836088146,0.100840510682596));
#10626=CARTESIAN_POINT('Ctrl Pts',(11.4,1.45718524058191,0.));
#10627=CARTESIAN_POINT('',(11.4,1.32241589772268,0.7));
#10628=CARTESIAN_POINT('Ctrl Pts',(11.3999999999682,1.32241589773435,0.7));
#10629=CARTESIAN_POINT('Ctrl Pts',(11.4000000023735,1.33035873561384,0.69999999792071));
#10630=CARTESIAN_POINT('Ctrl Pts',(11.3999980827719,1.33823923135401,0.699006238562837));
#10631=CARTESIAN_POINT('Ctrl Pts',(11.3999964146773,1.34591623266897,0.697118452648154));
#10632=CARTESIAN_POINT('Ctrl Pts',(11.3999954805754,1.35021521026861,0.696061327733467));
#10633=CARTESIAN_POINT('Ctrl Pts',(11.3999946303028,1.35445042327231,0.694722827332644));
#10634=CARTESIAN_POINT('Ctrl Pts',(11.3999940855437,1.35859537550353,0.6931136259882));
#10635=CARTESIAN_POINT('Ctrl Pts',(11.3999931076272,1.36603612757745,0.690224891070856));
#10636=CARTESIAN_POINT('Ctrl Pts',(11.3999932937992,1.3731074395729,0.686497549823264));
#10637=CARTESIAN_POINT('Ctrl Pts',(11.3999945206258,1.37966241828116,0.682010734965951));
#10638=CARTESIAN_POINT('Ctrl Pts',(11.3999951957832,1.38326980879772,0.679541513617388));
#10639=CARTESIAN_POINT('Ctrl Pts',(11.399996159718,1.38672054258633,0.67684140394947));
#10640=CARTESIAN_POINT('Ctrl Pts',(11.3999970106794,1.38998612808193,0.67391813047908));
#10641=CARTESIAN_POINT('Ctrl Pts',(11.399997834674,1.39314822810011,0.671087494715186));
#10642=CARTESIAN_POINT('Ctrl Pts',(11.3999985616145,1.39611771109305,0.668064564866167));
#10643=CARTESIAN_POINT('Ctrl Pts',(11.3999985600482,1.39887227052748,0.664860274403491));
#10644=CARTESIAN_POINT('Ctrl Pts',(11.3999985571253,1.40401282028653,0.65888043807832));
#10645=CARTESIAN_POINT('Ctrl Pts',(11.3999962993541,1.40840780441339,0.652270325570232));
#10646=CARTESIAN_POINT('Ctrl Pts',(11.399995545677,1.411994629421,0.6451936465425));
#10647=CARTESIAN_POINT('Ctrl Pts',(11.3999954685939,1.41236147527551,0.644469872631166));
#10648=CARTESIAN_POINT('Ctrl Pts',(11.3999954033687,1.41271982702329,0.643741199273148));
#10649=CARTESIAN_POINT('Ctrl Pts',(11.399995351278,1.41306958904162,0.643007791034547));
#10650=CARTESIAN_POINT('Ctrl Pts',(11.3999948427782,1.41648390439843,0.635848388696429));
#10651=CARTESIAN_POINT('Ctrl Pts',(11.3999960181446,1.41904356023948,0.628323447569199));
#10652=CARTESIAN_POINT('Ctrl Pts',(11.3999977140636,1.42069349507095,0.620600117586001));
#10653=CARTESIAN_POINT('Ctrl Pts',(11.3999987928026,1.4217429844709,0.615687467222433));
#10654=CARTESIAN_POINT('Ctrl Pts',(11.4,1.42242354791745,0.610693903223035));
#10655=CARTESIAN_POINT('Ctrl Pts',(11.4,1.42271022042989,0.605660349289938));
#10656=CARTESIAN_POINT('',(11.4,-1.32241589772233,0.7));
#10657=CARTESIAN_POINT('',(11.4,-0.768899768518519,0.7));
#10658=CARTESIAN_POINT('Ctrl Pts',(11.4,-1.4227102204299,0.605660349289938));
#10659=CARTESIAN_POINT('Ctrl Pts',(11.4,-1.42225988230954,0.613567634148305));
#10660=CARTESIAN_POINT('Ctrl Pts',(11.399997277834,-1.42084002197897,0.621378952482038));
#10661=CARTESIAN_POINT('Ctrl Pts',(11.3999960666067,-1.41853584574224,0.62893480307212));
#10662=CARTESIAN_POINT('Ctrl Pts',(11.3999954054252,-1.41727804822547,0.633059370437125));
#10663=CARTESIAN_POINT('Ctrl Pts',(11.399995101512,-1.41575577202439,0.637107840337094));
#10664=CARTESIAN_POINT('Ctrl Pts',(11.3999952458732,-1.4139766528271,0.641052464558972));
#10665=CARTESIAN_POINT('Ctrl Pts',(11.3999955106959,-1.41071295596475,0.648288661951321));
#10666=CARTESIAN_POINT('Ctrl Pts',(11.3999975070228,-1.40662392062869,0.655096264526915));
#10667=CARTESIAN_POINT('Ctrl Pts',(11.3999983091255,-1.40177626405188,0.661313589686923));
#10668=CARTESIAN_POINT('Ctrl Pts',(11.3999984645713,-1.40083679843637,0.66251849418371));
#10669=CARTESIAN_POINT('Ctrl Pts',(11.3999985618942,-1.3998687022723,0.663701157110503));
#10670=CARTESIAN_POINT('Ctrl Pts',(11.3999985615247,-1.39887227038638,0.664860274403572));
#10671=CARTESIAN_POINT('Ctrl Pts',(11.3999985608543,-1.39706426040285,0.666963474499402));
#10672=CARTESIAN_POINT('Ctrl Pts',(11.3999982409398,-1.39516298427334,0.668989190735049));
#10673=CARTESIAN_POINT('Ctrl Pts',(11.3999977953094,-1.39317470503404,0.670934323115149));
#10674=CARTESIAN_POINT('Ctrl Pts',(11.3999965209597,-1.38748891009577,0.67649673287249));
#10675=CARTESIAN_POINT('Ctrl Pts',(11.3999944455422,-1.38115857071774,0.681340422576046));
#10676=CARTESIAN_POINT('Ctrl Pts',(11.3999937508435,-1.37434881732181,0.685413525744465));
#10677=CARTESIAN_POINT('Ctrl Pts',(11.3999933041982,-1.36997059693002,0.688032261301096));
#10678=CARTESIAN_POINT('Ctrl Pts',(11.3999933336943,-1.3653932120823,0.69033179581025));
#10679=CARTESIAN_POINT('Ctrl Pts',(11.399993839827,-1.36065445462682,0.69228884175444));
#10680=CARTESIAN_POINT('Ctrl Pts',(11.3999946245508,-1.35330733883187,0.695323106179894));
#10681=CARTESIAN_POINT('Ctrl Pts',(11.3999965692242,-1.34565642326237,0.69750197024776));
#10682=CARTESIAN_POINT('Ctrl Pts',(11.3999981510416,-1.33784990929195,0.698756936804364));
#10683=CARTESIAN_POINT('Ctrl Pts',(11.399999182603,-1.33275899381189,0.699575346749464));
#10684=CARTESIAN_POINT('Ctrl Pts',(11.4000000015384,-1.32760128986121,0.699999998642559));
#10685=CARTESIAN_POINT('Ctrl Pts',(11.3999999999682,-1.32241589773435,0.7));
#10686=CARTESIAN_POINT('Ctrl Pts',(11.227882892666,-1.47337141465794,-0.000640335460849732));
#10687=CARTESIAN_POINT('Ctrl Pts',(11.218588765022,-1.46278323638644,0.201451598614313));
#10688=CARTESIAN_POINT('Ctrl Pts',(11.2092944683555,-1.45219508216535,0.40354352620373));
#10689=CARTESIAN_POINT('Ctrl Pts',(11.2000000000001,-1.44160695250309,0.60563544721184));
#10690=CARTESIAN_POINT('Ctrl Pts',(10.1843397214697,-1.57034855377304,-0.000384310983874139));
#10691=CARTESIAN_POINT('Ctrl Pts',(10.1768953195658,-1.55975965902304,0.201708049868595));
#10692=CARTESIAN_POINT('Ctrl Pts',(10.1694507716805,-1.54917076711515,0.403800406245857));
#10693=CARTESIAN_POINT('Ctrl Pts',(10.1620060668616,-1.53858190981164,0.605892758286982));
#10694=CARTESIAN_POINT('Ctrl Pts',(9.14170648965309,-1.65016851777514,-0.000148134864058495));
#10695=CARTESIAN_POINT('Ctrl Pts',(9.13611341817177,-1.63957870617509,0.201944615677573));
#10696=CARTESIAN_POINT('Ctrl Pts',(9.13052023035058,-1.6289888900612,0.404037363603497));
#10697=CARTESIAN_POINT('Ctrl Pts',(9.124926910836,-1.6183991014662,0.606130109186173));
#10698=CARTESIAN_POINT('Ctrl Pts',(8.1,-1.69866351109718,1.00613961606655E-16));
#10699=CARTESIAN_POINT('Ctrl Pts',(8.09625995443094,-1.68807302815665,0.202092993803311));
#10700=CARTESIAN_POINT('Ctrl Pts',(8.09251982249141,-1.67748255132318,0.404185986335255));
#10701=CARTESIAN_POINT('Ctrl Pts',(8.08877960280056,-1.66689208072706,0.606278977577217));
#10702=CARTESIAN_POINT('Ctrl Pts',(8.1,-1.66641703131627,0.605314487869832));
#10703=CARTESIAN_POINT('Ctrl Pts',(9.13548525483003,-1.617718421277,0.605389190939432));
#10704=CARTESIAN_POINT('Ctrl Pts',(10.168822041161,-1.53796707615457,0.605507632815633));
#10705=CARTESIAN_POINT('Ctrl Pts',(11.2000000000893,-1.44160695345912,0.605635447210802));
#10706=CARTESIAN_POINT('Ctrl Pts',(11.7095939787209,-1.42740645209206,-7.69249563980189E-5));
#10707=CARTESIAN_POINT('Ctrl Pts',(11.6994545874061,-1.41682738380082,0.201847033339061));
#10708=CARTESIAN_POINT('Ctrl Pts',(11.6893150192885,-1.40624834198077,0.403770984173611));
#10709=CARTESIAN_POINT('Ctrl Pts',(11.6791752715866,-1.39566932719028,0.605694927437301));
#10710=CARTESIAN_POINT('Ctrl Pts',(11.6063871276792,-1.43748358609578,-5.11721697277706E-5));
#10711=CARTESIAN_POINT('Ctrl Pts',(11.596430427176,-1.42690445239132,0.201872829148883));
#10712=CARTESIAN_POINT('Ctrl Pts',(11.5864735514701,-1.41632534465399,0.403796823219986));
#10713=CARTESIAN_POINT('Ctrl Pts',(11.5765164978042,-1.40574626343445,0.605720809936841));
#10714=CARTESIAN_POINT('Ctrl Pts',(11.5031891278894,-1.4474144288224,-2.55082377288765E-5));
#10715=CARTESIAN_POINT('Ctrl Pts',(11.4934151336386,-1.43683522760458,0.201898535909597));
#10716=CARTESIAN_POINT('Ctrl Pts',(11.4836409658656,-1.42625605183456,0.40382257302165));
#10717=CARTESIAN_POINT('Ctrl Pts',(11.4738666218385,-1.41567690205216,0.605746602994839));
#10718=CARTESIAN_POINT('Ctrl Pts',(11.4,-1.45718524058191,-5.20417042793042E-18));
#10719=CARTESIAN_POINT('Ctrl Pts',(11.3904087275488,-1.44660597001679,0.201924086674796));
#10720=CARTESIAN_POINT('Ctrl Pts',(11.3808172833376,-1.43602672436683,0.403848166524883));
#10721=CARTESIAN_POINT('Ctrl Pts',(11.3712256646606,-1.42544750415802,0.605772239449758));
#10722=CARTESIAN_POINT('',(11.6778970386953,-1.39579479040469,0.605695249702977));
#10723=CARTESIAN_POINT('Ctrl Pts',(11.4,-1.4227102204299,0.605660349289938));
#10724=CARTESIAN_POINT('Ctrl Pts',(11.4926474653491,-1.41386220753305,0.605671932550561));
#10725=CARTESIAN_POINT('Ctrl Pts',(11.585279512325,-1.40488700096013,0.605683574233495));
#10726=CARTESIAN_POINT('Ctrl Pts',(11.6778970386953,-1.39579479040469,0.605695249702977));
#10727=CARTESIAN_POINT('Ctrl Pts',(11.6778970386953,-1.39579479040469,0.605695249702977));
#10728=CARTESIAN_POINT('Ctrl Pts',(11.6884613130147,-1.40633044792991,0.403796817797553));
#10729=CARTESIAN_POINT('Ctrl Pts',(11.6990256725537,-1.41686632615463,0.201898401304098));
#10730=CARTESIAN_POINT('Ctrl Pts',(11.7095901160181,-1.42740242188993,5.19332840620557E-17));
#10731=CARTESIAN_POINT('Ctrl Pts',(11.2,-1.34133050917871,0.7));
#10732=CARTESIAN_POINT('Ctrl Pts',(10.1668086441106,-1.43797263608903,0.7));
#10733=CARTESIAN_POINT('Ctrl Pts',(9.13190264019122,-1.51792184128158,0.7));
#10734=CARTESIAN_POINT('Ctrl Pts',(8.09530923905977,-1.56666858280461,0.7));
#10735=CARTESIAN_POINT('Ctrl Pts',(11.2026864299662,-1.37005086445236,0.7));
#10736=CARTESIAN_POINT('Ctrl Pts',(10.1691860218014,-1.46674693471719,0.700000910790016));
#10737=CARTESIAN_POINT('Ctrl Pts',(9.13384227773975,-1.54675516497,0.699999464833944));
#10738=CARTESIAN_POINT('Ctrl Pts',(8.09666712422266,-1.59554384206015,0.700000000000001));
#10739=CARTESIAN_POINT('Ctrl Pts',(11.2073428085028,-1.4198317437391,0.676744232988519));
#10740=CARTESIAN_POINT('Ctrl Pts',(10.1733099382853,-1.51661799675652,0.676702307311825));
#10741=CARTESIAN_POINT('Ctrl Pts',(9.13719745543551,-1.59672983278297,0.676663906627884));
#10742=CARTESIAN_POINT('Ctrl Pts',(8.09902054834098,-1.64558911349573,0.676639354455264));
#10743=CARTESIAN_POINT('Ctrl Pts',(11.2091847227485,-1.43952346553595,0.627236497176141));
#10744=CARTESIAN_POINT('Ctrl Pts',(10.1749352046592,-1.53629892039422,0.62712791425818));
#10745=CARTESIAN_POINT('Ctrl Pts',(9.13852107143019,-1.61640633519008,0.627027713743691));
#10746=CARTESIAN_POINT('Ctrl Pts',(8.0999458765183,-1.66526610220338,0.626964226563296));
#10747=CARTESIAN_POINT('Ctrl Pts',(11.209298290232,-1.4407376041935,0.605636599993194));
#10748=CARTESIAN_POINT('Ctrl Pts',(10.1750338985877,-1.53748737250229,0.605508345221004));
#10749=CARTESIAN_POINT('Ctrl Pts',(9.13859765097935,-1.61757204607208,0.605389415477198));
#10750=CARTESIAN_POINT('Ctrl Pts',(8.1,-1.66641703131627,0.605314487869832));
#10751=CARTESIAN_POINT('Ctrl Pts',(11.2,-1.34133050917871,0.7));
#10752=CARTESIAN_POINT('Ctrl Pts',(10.16836710286,-1.43782686176815,0.7));
#10753=CARTESIAN_POINT('Ctrl Pts',(9.13502472651537,-1.51768061363633,0.7));
#10754=CARTESIAN_POINT('Ctrl Pts',(8.09999999865516,-1.56644778212326,0.7));
#10755=CARTESIAN_POINT('Ctrl Pts',(11.6681436286308,-1.2964346619681,0.7));
#10756=CARTESIAN_POINT('Ctrl Pts',(11.5756099286391,-1.3055179747114,0.7));
#10757=CARTESIAN_POINT('Ctrl Pts',(11.4830653488871,-1.31448403714215,0.7));
#10758=CARTESIAN_POINT('Ctrl Pts',(11.3905090053564,-1.32332268868375,0.7));
#10759=CARTESIAN_POINT('Ctrl Pts',(11.6709605510772,-1.32513126902304,0.700000000000001));
#10760=CARTESIAN_POINT('Ctrl Pts',(11.5784027531871,-1.33421922733773,0.700000082825348));
#10761=CARTESIAN_POINT('Ctrl Pts',(11.4858332859074,-1.34318985044544,0.699999917777441));
#10762=CARTESIAN_POINT('Ctrl Pts',(11.3932507170007,-1.35203326785046,0.7));
#10763=CARTESIAN_POINT('Ctrl Pts',(11.6758431636759,-1.37487151491717,0.67676311428296));
#10764=CARTESIAN_POINT('Ctrl Pts',(11.583243842395,-1.38396722707511,0.676759299309384));
#10765=CARTESIAN_POINT('Ctrl Pts',(11.4906306781253,-1.39294591144353,0.676755553516685));
#10766=CARTESIAN_POINT('Ctrl Pts',(11.3980029235659,-1.40179729139028,0.67675176769038));
#10767=CARTESIAN_POINT('Ctrl Pts',(11.6777767156198,-1.39456903283364,0.627286048421068));
#10768=CARTESIAN_POINT('Ctrl Pts',(11.5851604051362,-1.40366358810601,0.627276165220861));
#10769=CARTESIAN_POINT('Ctrl Pts',(11.4925297866457,-1.41264104586547,0.627266369072496));
#10770=CARTESIAN_POINT('Ctrl Pts',(11.3998836071583,-1.4214913811319,0.627256563056779));
#10771=CARTESIAN_POINT('Ctrl Pts',(11.6778970386953,-1.39579479040469,0.605695249702977));
#10772=CARTESIAN_POINT('Ctrl Pts',(11.585279512325,-1.40488700096013,0.605683574233495));
#10773=CARTESIAN_POINT('Ctrl Pts',(11.4926474653491,-1.41386220753305,0.605671932550561));
#10774=CARTESIAN_POINT('Ctrl Pts',(11.4,-1.4227102204299,0.605660349289938));
#10775=CARTESIAN_POINT('',(11.6681436286308,-1.2964346619681,0.7));
#10776=CARTESIAN_POINT('Ctrl Pts',(11.6681436286308,-1.2964346619681,0.7));
#10777=CARTESIAN_POINT('Ctrl Pts',(11.5787728332608,-1.30520749699507,0.7));
#10778=CARTESIAN_POINT('Ctrl Pts',(11.4893918891838,-1.31387096021207,0.7));
#10779=CARTESIAN_POINT('Ctrl Pts',(11.3999999999682,-1.32241589773435,0.7));
#10780=CARTESIAN_POINT('Origin',(11.6681436286308,-1.2964346619681,0.6));
#10781=CARTESIAN_POINT('Origin',(6.08012166120517,1.06778195214465E-16,
0.7));
#10782=CARTESIAN_POINT('Ctrl Pts',(8.0999999986552,1.56644778212326,0.7));
#10783=CARTESIAN_POINT('Ctrl Pts',(9.13502472651542,1.51768061363633,0.7));
#10784=CARTESIAN_POINT('Ctrl Pts',(10.16836710286,1.43782686176815,0.7));
#10785=CARTESIAN_POINT('Ctrl Pts',(11.2,1.34133050917871,0.7));
#10786=CARTESIAN_POINT('Origin',(6.08012166120517,1.06778195214465E-16,
0.7));
#10787=CARTESIAN_POINT('',(11.6681436286308,1.2964346619681,0.7));
#10788=CARTESIAN_POINT('Ctrl Pts',(11.3999999999682,1.32241589773435,0.7));
#10789=CARTESIAN_POINT('Ctrl Pts',(11.4893918891837,1.31387096021208,0.7));
#10790=CARTESIAN_POINT('Ctrl Pts',(11.5787728332608,1.30520749699508,0.7));
#10791=CARTESIAN_POINT('Ctrl Pts',(11.6681436286308,1.2964346619681,0.7));
#10792=CARTESIAN_POINT('',(11.6681436286308,0.8,0.7));
#10793=CARTESIAN_POINT('Ctrl Pts',(8.09530923905978,1.56666858280461,0.7));
#10794=CARTESIAN_POINT('Ctrl Pts',(9.13190264019124,1.51792184128158,0.7));
#10795=CARTESIAN_POINT('Ctrl Pts',(10.1668086441106,1.43797263608903,0.7));
#10796=CARTESIAN_POINT('Ctrl Pts',(11.2,1.34133050917871,0.7));
#10797=CARTESIAN_POINT('Ctrl Pts',(8.09666712422266,1.59554384206015,0.700000000000001));
#10798=CARTESIAN_POINT('Ctrl Pts',(9.13384227773977,1.54675516497,0.699999464833944));
#10799=CARTESIAN_POINT('Ctrl Pts',(10.1691860218013,1.46674693471719,0.700000910790016));
#10800=CARTESIAN_POINT('Ctrl Pts',(11.2026864299662,1.37005086445236,0.7));
#10801=CARTESIAN_POINT('Ctrl Pts',(8.09902054834099,1.64558911349573,0.676639354455264));
#10802=CARTESIAN_POINT('Ctrl Pts',(9.13719745543553,1.59672983278297,0.676663906627884));
#10803=CARTESIAN_POINT('Ctrl Pts',(10.1733099382853,1.51661799675652,0.676702307311825));
#10804=CARTESIAN_POINT('Ctrl Pts',(11.2073428085028,1.4198317437391,0.676744232988519));
#10805=CARTESIAN_POINT('Ctrl Pts',(8.0999458765183,1.66526610220338,0.626964226563296));
#10806=CARTESIAN_POINT('Ctrl Pts',(9.1385210714302,1.61640633519008,0.627027713743691));
#10807=CARTESIAN_POINT('Ctrl Pts',(10.1749352046592,1.53629892039423,0.62712791425818));
#10808=CARTESIAN_POINT('Ctrl Pts',(11.2091847227485,1.43952346553595,0.627236497176141));
#10809=CARTESIAN_POINT('Ctrl Pts',(8.1,1.66641703131627,0.605314487869832));
#10810=CARTESIAN_POINT('Ctrl Pts',(9.13859765097937,1.61757204607208,0.605389415477198));
#10811=CARTESIAN_POINT('Ctrl Pts',(10.1750338985877,1.53748737250229,0.605508345221004));
#10812=CARTESIAN_POINT('Ctrl Pts',(11.209298290232,1.4407376041935,0.605636599993194));
#10813=CARTESIAN_POINT('Ctrl Pts',(11.2000000000893,1.44160695345912,0.605635447210802));
#10814=CARTESIAN_POINT('Ctrl Pts',(10.168822041161,1.53796707615457,0.605507632815633));
#10815=CARTESIAN_POINT('Ctrl Pts',(9.13548525483005,1.617718421277,0.605389190939432));
#10816=CARTESIAN_POINT('Ctrl Pts',(8.1,1.66641703131627,0.605314487869832));
#10817=CARTESIAN_POINT('Ctrl Pts',(8.1,1.69866351109859,-2.6441702993818E-11));
#10818=CARTESIAN_POINT('Ctrl Pts',(8.09625995443078,1.68807302815759,0.202092993785684));
#10819=CARTESIAN_POINT('Ctrl Pts',(8.09251982249108,1.67748255132366,0.404185986326441));
#10820=CARTESIAN_POINT('Ctrl Pts',(8.08877960280008,1.66689208072708,0.606278977577217));
#10821=CARTESIAN_POINT('Ctrl Pts',(9.14170648965349,1.65016851777655,-0.00014813489050026));
#10822=CARTESIAN_POINT('Ctrl Pts',(9.13611341817193,1.63957870617604,0.201944615659945));
#10823=CARTESIAN_POINT('Ctrl Pts',(9.1305202303505,1.62898889006169,0.404037363594684));
#10824=CARTESIAN_POINT('Ctrl Pts',(9.12492691083567,1.61839910146622,0.606130109186173));
#10825=CARTESIAN_POINT('Ctrl Pts',(10.1843397214705,1.57034855377444,-0.000384311010315772));
#10826=CARTESIAN_POINT('Ctrl Pts',(10.1768953195662,1.55975965902398,0.201708049850968));
#10827=CARTESIAN_POINT('Ctrl Pts',(10.1694507716807,1.54917076711562,0.403800406237042));
#10828=CARTESIAN_POINT('Ctrl Pts',(10.1620060668615,1.53858190981166,0.605892758286982));
#10829=CARTESIAN_POINT('Ctrl Pts',(11.2278828926672,1.47337141465933,-0.000640335487291374));
#10830=CARTESIAN_POINT('Ctrl Pts',(11.2185887650228,1.46278323638736,0.201451598596686));
#10831=CARTESIAN_POINT('Ctrl Pts',(11.2092944683559,1.45219508216582,0.403543526194916));
#10832=CARTESIAN_POINT('Ctrl Pts',(11.2000000000001,1.44160695250309,0.60563544721184));
#10833=CARTESIAN_POINT('Ctrl Pts',(11.4,1.45718524058191,-1.37043154602168E-16));
#10834=CARTESIAN_POINT('Ctrl Pts',(11.3904087275488,1.44660597001679,0.201924086674796));
#10835=CARTESIAN_POINT('Ctrl Pts',(11.3808172833376,1.43602672436683,0.403848166524884));
#10836=CARTESIAN_POINT('Ctrl Pts',(11.3712256646606,1.42544750415802,0.605772239449759));
#10837=CARTESIAN_POINT('Ctrl Pts',(11.5031891278894,1.4474144288224,-2.55082377290153E-5));
#10838=CARTESIAN_POINT('Ctrl Pts',(11.4934151336386,1.43683522760458,0.201898535909598));
#10839=CARTESIAN_POINT('Ctrl Pts',(11.4836409658656,1.42625605183455,0.40382257302165));
#10840=CARTESIAN_POINT('Ctrl Pts',(11.4738666218385,1.41567690205216,0.605746602994839));
#10841=CARTESIAN_POINT('Ctrl Pts',(11.6063871276792,1.43748358609579,-5.1172169727805E-5));
#10842=CARTESIAN_POINT('Ctrl Pts',(11.596430427176,1.42690445239132,0.201872829148883));
#10843=CARTESIAN_POINT('Ctrl Pts',(11.5864735514701,1.41632534465399,0.403796823219986));
#10844=CARTESIAN_POINT('Ctrl Pts',(11.5765164978042,1.40574626343445,0.605720809936842));
#10845=CARTESIAN_POINT('Ctrl Pts',(11.7095939787209,1.42740645209206,-7.69249563980588E-5));
#10846=CARTESIAN_POINT('Ctrl Pts',(11.6994545874061,1.41682738380082,0.201847033339061));
#10847=CARTESIAN_POINT('Ctrl Pts',(11.6893150192885,1.40624834198077,0.403770984173611));
#10848=CARTESIAN_POINT('Ctrl Pts',(11.6791752715866,1.39566932719028,0.605694927437301));
#10849=CARTESIAN_POINT('',(11.6778970386953,1.39579479040469,0.605695249702977));
#10850=CARTESIAN_POINT('Ctrl Pts',(11.7095901160181,1.42740242188993,2.01986864734049E-16));
#10851=CARTESIAN_POINT('Ctrl Pts',(11.6990256725537,1.41686632615463,0.201898401304098));
#10852=CARTESIAN_POINT('Ctrl Pts',(11.6884613130147,1.40633044792991,0.403796817797553));
#10853=CARTESIAN_POINT('Ctrl Pts',(11.6778970386953,1.39579479040469,0.605695249702978));
#10854=CARTESIAN_POINT('Ctrl Pts',(11.6778970386953,1.39579479040469,0.605695249702977));
#10855=CARTESIAN_POINT('Ctrl Pts',(11.585279512325,1.40488700096013,0.605683574233495));
#10856=CARTESIAN_POINT('Ctrl Pts',(11.4926474653491,1.41386220753305,0.605671932550561));
#10857=CARTESIAN_POINT('Ctrl Pts',(11.4,1.4227102204299,0.605660349289938));
#10858=CARTESIAN_POINT('Origin',(7.9,1.7737037037037,0.));
#10859=CARTESIAN_POINT('',(7.9,-1.67543132363858,0.605300614462415));
#10860=CARTESIAN_POINT('Ctrl Pts',(7.9,-1.67543132363858,0.605300614462415));
#10861=CARTESIAN_POINT('Ctrl Pts',(7.9,-1.68078196203297,0.504592238472094));
#10862=CARTESIAN_POINT('Ctrl Pts',(7.9,-1.68613236521525,0.403883028813119));
#10863=CARTESIAN_POINT('Ctrl Pts',(7.9,-1.69685110017509,0.202116711316755));
#10864=CARTESIAN_POINT('Ctrl Pts',(7.9,-1.70221951791351,0.10105794916591));
#10865=CARTESIAN_POINT('Ctrl Pts',(7.9,-1.70758761671949,0.));
#10866=CARTESIAN_POINT('',(7.9,-1.57547905376932,0.7));
#10867=CARTESIAN_POINT('Ctrl Pts',(7.9,-1.57547905376882,0.7));
#10868=CARTESIAN_POINT('Ctrl Pts',(7.9,-1.58339333479856,0.700000000000001));
#10869=CARTESIAN_POINT('Ctrl Pts',(7.89999913038498,-1.59124411312484,0.699006032637452));
#10870=CARTESIAN_POINT('Ctrl Pts',(7.89999837104309,-1.59889106951376,0.697118831203047));
#10871=CARTESIAN_POINT('Ctrl Pts',(7.89999794343345,-1.6031973145812,0.696056087876834));
#10872=CARTESIAN_POINT('Ctrl Pts',(7.89999755365678,-1.60743898057435,0.694709047589066));
#10873=CARTESIAN_POINT('Ctrl Pts',(7.89999730661842,-1.61158931211603,0.693088720937666));
#10874=CARTESIAN_POINT('Ctrl Pts',(7.89999686465941,-1.6190143793929,0.690189908089508));
#10875=CARTESIAN_POINT('Ctrl Pts',(7.89999696143539,-1.626066934352,0.686450944759811));
#10876=CARTESIAN_POINT('Ctrl Pts',(7.89999752554231,-1.63260082031789,0.681953255064161));
#10877=CARTESIAN_POINT('Ctrl Pts',(7.89999783650325,-1.63620259020663,0.679473927540052));
#10878=CARTESIAN_POINT('Ctrl Pts',(7.89999827825103,-1.63964648551863,0.676763160200805));
#10879=CARTESIAN_POINT('Ctrl Pts',(7.89999867021687,-1.64290407802379,0.673829034208746));
#10880=CARTESIAN_POINT('Ctrl Pts',(7.89999905115172,-1.64606999298761,0.670977482527793));
#10881=CARTESIAN_POINT('Ctrl Pts',(7.89999938859403,-1.64904076201529,0.667932171841817));
#10882=CARTESIAN_POINT('Ctrl Pts',(7.89999938783828,-1.6517939440564,0.66470449824639));
#10883=CARTESIAN_POINT('Ctrl Pts',(7.89999938643498,-1.65690611124346,0.658711285012161));
#10884=CARTESIAN_POINT('Ctrl Pts',(7.89999834643869,-1.661271022418,0.652090721578155));
#10885=CARTESIAN_POINT('Ctrl Pts',(7.89999799057748,-1.66482884904143,0.645008203309728));
#10886=CARTESIAN_POINT('Ctrl Pts',(7.89999795399159,-1.66519462718329,0.644280053614395));
#10887=CARTESIAN_POINT('Ctrl Pts',(7.89999792287445,-1.66555183396469,0.643547001244109));
#10888=CARTESIAN_POINT('Ctrl Pts',(7.89999789784292,-1.66590037542058,0.642809214685104));
#10889=CARTESIAN_POINT('Ctrl Pts',(7.89999765441981,-1.66928982250308,0.635634491398386));
#10890=CARTESIAN_POINT('Ctrl Pts',(7.89999817709027,-1.67182454272713,0.628096763436417));
#10891=CARTESIAN_POINT('Ctrl Pts',(7.8999989464625,-1.67345106343068,0.620364350320046));
#10892=CARTESIAN_POINT('Ctrl Pts',(7.89999943944948,-1.67449328136075,0.615409688768565));
#10893=CARTESIAN_POINT('Ctrl Pts',(7.89999999630063,-1.67516175160204,0.610374426093907));
#10894=CARTESIAN_POINT('Ctrl Pts',(7.89999999769359,-1.67543132314592,0.605300614465834));
#10895=CARTESIAN_POINT('',(7.9,1.57547905376882,0.7));
#10896=CARTESIAN_POINT('',(7.9,0.886851851851852,0.7));
#10897=CARTESIAN_POINT('',(7.9,1.67543132363858,0.605300614462415));
#10898=CARTESIAN_POINT('Ctrl Pts',(7.89999999769359,1.67543132314592,0.605300614465834));
#10899=CARTESIAN_POINT('Ctrl Pts',(7.89999999552123,1.67501091691767,0.613213400729193));
#10900=CARTESIAN_POINT('Ctrl Pts',(7.89999875799714,1.67362284400845,0.621034919585595));
#10901=CARTESIAN_POINT('Ctrl Pts',(7.89999821041927,1.67135120200026,0.628604813990272));
#10902=CARTESIAN_POINT('Ctrl Pts',(7.89999790518813,1.67008494211401,0.632824428521627));
#10903=CARTESIAN_POINT('Ctrl Pts',(7.89999777089825,1.66854314417455,0.636965893954691));
#10904=CARTESIAN_POINT('Ctrl Pts',(7.89999784944871,1.66673368022774,0.640999456224326));
#10905=CARTESIAN_POINT('Ctrl Pts',(7.89999799035603,1.66348778281681,0.648235040746992));
#10906=CARTESIAN_POINT('Ctrl Pts',(7.8999989183875,1.65941887886545,0.655045206964536));
#10907=CARTESIAN_POINT('Ctrl Pts',(7.89999927807636,1.65459101651367,0.661266862646797));
#10908=CARTESIAN_POINT('Ctrl Pts',(7.89999934554656,1.65368540929837,0.662433916689859));
#10909=CARTESIAN_POINT('Ctrl Pts',(7.89999938740919,1.65275296801062,0.663580193269421));
#10910=CARTESIAN_POINT('Ctrl Pts',(7.89999938728957,1.65179394408007,0.664704498246374));
#10911=CARTESIAN_POINT('Ctrl Pts',(7.89999938705343,1.64990069294102,0.666924037937161));
#10912=CARTESIAN_POINT('Ctrl Pts',(7.89999922461202,1.64790387543569,0.669057997255949));
#10913=CARTESIAN_POINT('Ctrl Pts',(7.89999900301747,1.64581073954063,0.671102663899023));
#10914=CARTESIAN_POINT('Ctrl Pts',(7.89999840121276,1.64012621790684,0.676655553128015));
#10915=CARTESIAN_POINT('Ctrl Pts',(7.89999746538644,1.63379824275617,0.681490110487894));
#10916=CARTESIAN_POINT('Ctrl Pts',(7.89999715581736,1.6269906793715,0.685552192443336));
#10917=CARTESIAN_POINT('Ctrl Pts',(7.89999695885968,1.62265949106942,0.688136618155352));
#10918=CARTESIAN_POINT('Ctrl Pts',(7.89999697413705,1.61813320929371,0.690407672840119));
#10919=CARTESIAN_POINT('Ctrl Pts',(7.89999720528031,1.61344832872307,0.692342105328139));
#10920=CARTESIAN_POINT('Ctrl Pts',(7.89999756646959,1.60612763680413,0.69536488980882));
#10921=CARTESIAN_POINT('Ctrl Pts',(7.89999845750109,1.59850458633822,0.69753330980446));
#10922=CARTESIAN_POINT('Ctrl Pts',(7.89999917312139,1.59072625322659,0.698777780766876));
#10923=CARTESIAN_POINT('Ctrl Pts',(7.8999996358458,1.58569673594883,0.699582463224842));
#10924=CARTESIAN_POINT('Ctrl Pts',(7.9,1.58060170040825,0.7));
#10925=CARTESIAN_POINT('Ctrl Pts',(7.9,1.57547905376882,0.7));
#10926=CARTESIAN_POINT('Ctrl Pts',(7.9,1.70758761671949,0.));
#10927=CARTESIAN_POINT('Ctrl Pts',(7.9,1.70221949782947,0.101058327261027));
#10928=CARTESIAN_POINT('Ctrl Pts',(7.9,1.69685105999395,0.202117467714));
#10929=CARTESIAN_POINT('Ctrl Pts',(7.9,1.68613232500772,0.403883785628764));
#10930=CARTESIAN_POINT('Ctrl Pts',(7.9,1.6807819419292,0.504592616860323));
#10931=CARTESIAN_POINT('Ctrl Pts',(7.9,1.67543132363858,0.605300614462415));
#10932=CARTESIAN_POINT('Ctrl Pts',(7.91019312999368,-1.70715886092982,-0.000134090250286965));
#10933=CARTESIAN_POINT('Ctrl Pts',(7.90679525219671,-1.69658223918655,0.201692187253877));
#10934=CARTESIAN_POINT('Ctrl Pts',(7.90339729501941,-1.68600562260833,0.40351846369823));
#10935=CARTESIAN_POINT('Ctrl Pts',(7.89999925719352,-1.67542901130525,0.605344739067286));
#10936=CARTESIAN_POINT('Ctrl Pts',(6.63535348802246,-1.76179300886274,3.38453142643293E-5));
#10937=CARTESIAN_POINT('Ctrl Pts',(6.63422081661327,-1.7512156246026,0.201860399405878));
#10938=CARTESIAN_POINT('Ctrl Pts',(6.6330881724013,-1.74063821514668,0.403686949685767));
#10939=CARTESIAN_POINT('Ctrl Pts',(6.63195543348167,-1.7300608292057,0.605513504373875));
#10940=CARTESIAN_POINT('Ctrl Pts',(5.36191629096386,-1.76821426310706,6.25694230841134E-5));
#10941=CARTESIAN_POINT('Ctrl Pts',(5.36305144950513,-1.75763653444312,0.201889164820622));
#10942=CARTESIAN_POINT('Ctrl Pts',(5.36418670601529,-1.74705878452761,0.403715755186214));
#10943=CARTESIAN_POINT('Ctrl Pts',(5.36532191986746,-1.73648104871457,0.605542351516859));
#10944=CARTESIAN_POINT('Ctrl Pts',(4.08978435919194,-1.70060618495018,-0.000163379468877527));
#10945=CARTESIAN_POINT('Ctrl Pts',(4.09318947412453,-1.69002991101751,0.201662855819258));
#10946=CARTESIAN_POINT('Ctrl Pts',(4.09659468720556,-1.67945364498778,0.403489089874722));
#10947=CARTESIAN_POINT('Ctrl Pts',(4.1,-1.66887738702936,0.605315322680078));
#10948=CARTESIAN_POINT('Ctrl Pts',(4.10000000006189,-1.66887738587128,0.605315322687833));
#10949=CARTESIAN_POINT('Ctrl Pts',(5.36600428635239,-1.73653511802878,0.605201749988751));
#10950=CARTESIAN_POINT('Ctrl Pts',(6.63469107356441,-1.72995836404769,0.605216415547347));
#10951=CARTESIAN_POINT('Ctrl Pts',(7.89999999997453,-1.67543132304763,0.605300614465986));
#10952=CARTESIAN_POINT('Ctrl Pts',(7.9,-1.57547905376882,0.7));
#10953=CARTESIAN_POINT('Ctrl Pts',(6.63400208894818,-1.63014048526579,0.7));
#10954=CARTESIAN_POINT('Ctrl Pts',(5.36531976402288,-1.63670020240541,0.7));
#10955=CARTESIAN_POINT('Ctrl Pts',(4.09999999999999,-1.56887583540973,0.7));
#10956=CARTESIAN_POINT('Ctrl Pts',(7.9012470621039,-1.60436190544783,0.700000000000001));
#10957=CARTESIAN_POINT('Ctrl Pts',(6.6345175325877,-1.65907137725265,0.700000604190856));
#10958=CARTESIAN_POINT('Ctrl Pts',(5.36490325870521,-1.66564852467601,0.700000815814724));
#10959=CARTESIAN_POINT('Ctrl Pts',(4.09845273665223,-1.59774131518914,0.699999999999999));
#10960=CARTESIAN_POINT('Ctrl Pts',(7.90340849276168,-1.6544221878571,0.676636720659303));
#10961=CARTESIAN_POINT('Ctrl Pts',(6.63541917043928,-1.70921256696412,0.676609005714152));
#10962=CARTESIAN_POINT('Ctrl Pts',(5.36416860778507,-1.71581908642683,0.67660414986632));
#10963=CARTESIAN_POINT('Ctrl Pts',(4.09577098158984,-1.64777167791894,0.676641578059328));
#10964=CARTESIAN_POINT('Ctrl Pts',(7.90425799286387,-1.67409721877663,0.626952737571144));
#10965=CARTESIAN_POINT('Ctrl Pts',(6.63576820027036,-1.72888861107585,0.626881076846221));
#10966=CARTESIAN_POINT('Ctrl Pts',(5.36388821219926,-1.73550154452763,0.626868555890157));
#10967=CARTESIAN_POINT('Ctrl Pts',(4.09471668402893,-1.66744047248441,0.626965338598652));
#10968=CARTESIAN_POINT('Ctrl Pts',(7.90430757201307,-1.67524550738887,0.605300901379154));
#10969=CARTESIAN_POINT('Ctrl Pts',(6.63578978311492,-1.73002023206136,0.605216330280387));
#10970=CARTESIAN_POINT('Ctrl Pts',(5.3638700255334,-1.7366305488338,0.605201579557148));
#10971=CARTESIAN_POINT('Ctrl Pts',(4.09465499692593,-1.6685912965035,0.605315802949303));
#10972=CARTESIAN_POINT('Ctrl Pts',(7.9,-1.57547905376882,0.7));
#10973=CARTESIAN_POINT('Ctrl Pts',(6.63400208894818,-1.63014048526579,0.7));
#10974=CARTESIAN_POINT('Ctrl Pts',(5.36531976402288,-1.63670020240541,0.7));
#10975=CARTESIAN_POINT('Ctrl Pts',(4.09999999999999,-1.56887583540973,0.7));
#10976=CARTESIAN_POINT('Origin',(6.08012166120517,1.06778195214465E-16,
0.7));
#10977=CARTESIAN_POINT('Ctrl Pts',(4.1,1.56887583540973,0.7));
#10978=CARTESIAN_POINT('Ctrl Pts',(5.36531976402291,1.63670020240541,0.7));
#10979=CARTESIAN_POINT('Ctrl Pts',(6.63400208894819,1.63014048526579,0.7));
#10980=CARTESIAN_POINT('Ctrl Pts',(7.9,1.57547905376882,0.7));
#10981=CARTESIAN_POINT('Ctrl Pts',(4.1,1.56887583540973,0.7));
#10982=CARTESIAN_POINT('Ctrl Pts',(5.36531976402291,1.63670020240541,0.7));
#10983=CARTESIAN_POINT('Ctrl Pts',(6.63400208894819,1.63014048526579,0.7));
#10984=CARTESIAN_POINT('Ctrl Pts',(7.9,1.57547905376882,0.7));
#10985=CARTESIAN_POINT('Ctrl Pts',(4.09845273665224,1.59774131518914,0.699999999999999));
#10986=CARTESIAN_POINT('Ctrl Pts',(5.36490325870523,1.66564852467601,0.700000815814725));
#10987=CARTESIAN_POINT('Ctrl Pts',(6.6345175325877,1.65907137725265,0.700000604190856));
#10988=CARTESIAN_POINT('Ctrl Pts',(7.9012470621039,1.60436190544783,0.700000000000001));
#10989=CARTESIAN_POINT('Ctrl Pts',(4.09577098158985,1.64777167791894,0.676641578059328));
#10990=CARTESIAN_POINT('Ctrl Pts',(5.36416860778509,1.71581908642683,0.67660414986632));
#10991=CARTESIAN_POINT('Ctrl Pts',(6.6354191704393,1.70921256696412,0.676609005714152));
#10992=CARTESIAN_POINT('Ctrl Pts',(7.90340849276168,1.6544221878571,0.676636720659302));
#10993=CARTESIAN_POINT('Ctrl Pts',(4.09471668402895,1.66744047248441,0.626965338598652));
#10994=CARTESIAN_POINT('Ctrl Pts',(5.36388821219928,1.73550154452763,0.626868555890157));
#10995=CARTESIAN_POINT('Ctrl Pts',(6.63576820027036,1.72888861107585,0.626881076846221));
#10996=CARTESIAN_POINT('Ctrl Pts',(7.90425799286387,1.67409721877663,0.626952737571144));
#10997=CARTESIAN_POINT('Ctrl Pts',(4.09465499692594,1.6685912965035,0.605315802949303));
#10998=CARTESIAN_POINT('Ctrl Pts',(5.36387002553342,1.7366305488338,0.605201579557148));
#10999=CARTESIAN_POINT('Ctrl Pts',(6.63578978311492,1.73002023206136,0.605216330280387));
#11000=CARTESIAN_POINT('Ctrl Pts',(7.90430757201307,1.67524550738887,0.605300901379154));
#11001=CARTESIAN_POINT('Ctrl Pts',(7.89999999997454,1.67543132304763,0.605300614465986));
#11002=CARTESIAN_POINT('Ctrl Pts',(6.63469107356441,1.72995836404769,0.605216415547348));
#11003=CARTESIAN_POINT('Ctrl Pts',(5.36600428635241,1.73653511802878,0.605201749988751));
#11004=CARTESIAN_POINT('Ctrl Pts',(4.10000000006189,1.66887738587128,0.605315322687833));
#11005=CARTESIAN_POINT('Ctrl Pts',(4.08978435969213,1.70060618339657,-0.000163349821525811));
#11006=CARTESIAN_POINT('Ctrl Pts',(4.093189474458,1.69002990998177,0.201662875584159));
#11007=CARTESIAN_POINT('Ctrl Pts',(4.0965946873723,1.67945364446992,0.403489099757173));
#11008=CARTESIAN_POINT('Ctrl Pts',(4.1,1.66887738702936,0.605315322680078));
#11009=CARTESIAN_POINT('Ctrl Pts',(5.36191629113061,1.76821426155324,6.25990704884337E-5));
#11010=CARTESIAN_POINT('Ctrl Pts',(5.3630514496163,1.75763653340724,0.201889184585558));
#11011=CARTESIAN_POINT('Ctrl Pts',(5.36418670607087,1.74705878400967,0.403715765068683));
#11012=CARTESIAN_POINT('Ctrl Pts',(5.36532191986745,1.73648104871457,0.605542351516858));
#11013=CARTESIAN_POINT('Ctrl Pts',(6.63535348785608,1.76179300730897,3.38749616628245E-5));
#11014=CARTESIAN_POINT('Ctrl Pts',(6.63422081650235,1.75121562356675,0.20186041917081));
#11015=CARTESIAN_POINT('Ctrl Pts',(6.63308817234583,1.74063821462875,0.403686959568233));
#11016=CARTESIAN_POINT('Ctrl Pts',(6.63195543348166,1.7300608292057,0.605513504373875));
#11017=CARTESIAN_POINT('Ctrl Pts',(7.91019312949454,1.70715885937616,-0.000134060602928919));
#11018=CARTESIAN_POINT('Ctrl Pts',(7.90679525186394,1.69658223815078,0.201692207018782));
#11019=CARTESIAN_POINT('Ctrl Pts',(7.90339729485302,1.68600562209044,0.403518473580683));
#11020=CARTESIAN_POINT('Ctrl Pts',(7.89999925719352,1.67542901130525,0.605344739067286));
#11021=CARTESIAN_POINT('Origin',(3.9,1.7662962962963,0.));
#11022=CARTESIAN_POINT('',(3.9,-1.657567947596,0.605334330700044));
#11023=CARTESIAN_POINT('Ctrl Pts',(3.9,-1.657567947596,0.605334330700044));
#11024=CARTESIAN_POINT('Ctrl Pts',(3.9,-1.66295505583237,0.504667750148195));
#11025=CARTESIAN_POINT('Ctrl Pts',(3.9,-1.66834175427306,0.404000185805616));
#11026=CARTESIAN_POINT('Ctrl Pts',(3.9,-1.67913790341918,0.202222727053817));
#11027=CARTESIAN_POINT('Ctrl Pts',(3.9,-1.68454745406112,0.101110889248462));
#11028=CARTESIAN_POINT('Ctrl Pts',(3.9,-1.68995649764597,0.));
#11029=CARTESIAN_POINT('',(3.9,-1.55753217754889,0.7));
#11030=CARTESIAN_POINT('Ctrl Pts',(3.89999999700315,-1.55753217437,0.7));
#11031=CARTESIAN_POINT('Ctrl Pts',(3.89999999197785,-1.56545359401377,0.699999998841372));
#11032=CARTESIAN_POINT('Ctrl Pts',(3.90000117861029,-1.57331197233837,0.699006163267487));
#11033=CARTESIAN_POINT('Ctrl Pts',(3.90000221019459,-1.58096665047841,0.697118921400131));
#11034=CARTESIAN_POINT('Ctrl Pts',(3.90000279139136,-1.58527931230009,0.696055645348449));
#11035=CARTESIAN_POINT('Ctrl Pts',(3.90000331912093,-1.58952737074567,0.694707745526415));
#11036=CARTESIAN_POINT('Ctrl Pts',(3.90000364796674,-1.59368396010392,0.693086194530447));
#11037=CARTESIAN_POINT('Ctrl Pts',(3.90000423564848,-1.60111221870485,0.690188313817561));
#11038=CARTESIAN_POINT('Ctrl Pts',(3.90000407815102,-1.60816848972648,0.686450841450731));
#11039=CARTESIAN_POINT('Ctrl Pts',(3.9000032813392,-1.6147063365644,0.681954558458482));
#11040=CARTESIAN_POINT('Ctrl Pts',(3.90000284137901,-1.61831621321653,0.679471932695374));
#11041=CARTESIAN_POINT('Ctrl Pts',(3.90000222202081,-1.62176776859012,0.67675708350434));
#11042=CARTESIAN_POINT('Ctrl Pts',(3.9000016760669,-1.6250323621476,0.673818036286869));
#11043=CARTESIAN_POINT('Ctrl Pts',(3.90000114791654,-1.62819049732732,0.670974831382826));
#11044=CARTESIAN_POINT('Ctrl Pts',(3.90000068451114,-1.63115458712464,0.667938911589952));
#11045=CARTESIAN_POINT('Ctrl Pts',(3.90000068976928,-1.6339023205034,0.664721489040691));
#11046=CARTESIAN_POINT('Ctrl Pts',(3.90000069956116,-1.63901923218135,0.658729908073458));
#11047=CARTESIAN_POINT('Ctrl Pts',(3.9000021571807,-1.64338878348726,0.652110283780478));
#11048=CARTESIAN_POINT('Ctrl Pts',(3.90000267296827,-1.64695081636755,0.645027851744832));
#11049=CARTESIAN_POINT('Ctrl Pts',(3.90000272641596,-1.64731992654249,0.644293945625623));
#11050=CARTESIAN_POINT('Ctrl Pts',(3.90000277224081,-1.64768032438231,0.643555049900053));
#11051=CARTESIAN_POINT('Ctrl Pts',(3.90000280957334,-1.64803191324525,0.642811337026806));
#11052=CARTESIAN_POINT('Ctrl Pts',(3.90000316967295,-1.65142324611312,0.635637680016741));
#11053=CARTESIAN_POINT('Ctrl Pts',(3.90000247513984,-1.65395957542788,0.628100801230905));
#11054=CARTESIAN_POINT('Ctrl Pts',(3.90000142932204,-1.65558732484325,0.62036898832433));
#11055=CARTESIAN_POINT('Ctrl Pts',(3.90000076044003,-1.65662839749185,0.615423891207338));
#11056=CARTESIAN_POINT('Ctrl Pts',(3.9,-1.65729694754734,0.61039839235075));
#11057=CARTESIAN_POINT('Ctrl Pts',(3.9,-1.657567947596,0.605334330700044));
#11058=CARTESIAN_POINT('',(3.9,1.55753217754922,0.7));
#11059=CARTESIAN_POINT('',(3.9,0.883148148148148,0.7));
#11060=CARTESIAN_POINT('',(3.9,1.657567947596,0.605334330700044));
#11061=CARTESIAN_POINT('Ctrl Pts',(3.9,1.657567947596,0.605334330700044));
#11062=CARTESIAN_POINT('Ctrl Pts',(3.9,1.65714453107083,0.613246533660879));
#11063=CARTESIAN_POINT('Ctrl Pts',(3.90000169450566,1.65575314729854,0.621067109624563));
#11064=CARTESIAN_POINT('Ctrl Pts',(3.900002426785,1.653477907766,0.628635640467799));
#11065=CARTESIAN_POINT('Ctrl Pts',(3.90000283370343,1.65221358571927,0.632841378048222));
#11066=CARTESIAN_POINT('Ctrl Pts',(3.90000300372053,1.65067534627202,0.636969322077829));
#11067=CARTESIAN_POINT('Ctrl Pts',(3.90000288278183,1.6488710006323,0.640990000951852));
#11068=CARTESIAN_POINT('Ctrl Pts',(3.90000266510116,1.6456233127241,0.64822692378658));
#11069=CARTESIAN_POINT('Ctrl Pts',(3.90000136145047,1.64155197609259,0.655037842274187));
#11070=CARTESIAN_POINT('Ctrl Pts',(3.9000008487987,1.63672139510901,0.661259788874982));
#11071=CARTESIAN_POINT('Ctrl Pts',(3.90000075195303,1.63580884415802,0.662435184403355));
#11072=CARTESIAN_POINT('Ctrl Pts',(3.90000069125178,1.63486906637168,0.663589490553999));
#11073=CARTESIAN_POINT('Ctrl Pts',(3.90000068992127,1.63390232051248,0.664721489040685));
#11074=CARTESIAN_POINT('Ctrl Pts',(3.90000068733544,1.63202347103487,0.666921503393101));
#11075=CARTESIAN_POINT('Ctrl Pts',(3.9000009071255,1.6300427915863,0.669037305429552));
#11076=CARTESIAN_POINT('Ctrl Pts',(3.90000121037842,1.62796736695056,0.671065303566633));
#11077=CARTESIAN_POINT('Ctrl Pts',(3.90000204102081,1.62228255539437,0.676620208836154));
#11078=CARTESIAN_POINT('Ctrl Pts',(3.90000335328325,1.61595386407616,0.681456575151491));
#11079=CARTESIAN_POINT('Ctrl Pts',(3.90000380482706,1.60914557515952,0.685520902406533));
#11080=CARTESIAN_POINT('Ctrl Pts',(3.90000409284089,1.60480295930069,0.688113302965514));
#11081=CARTESIAN_POINT('Ctrl Pts',(3.90000408819389,1.6002642541482,0.690390927291682));
#11082=CARTESIAN_POINT('Ctrl Pts',(3.90000378365133,1.59556629223371,0.692330537597694));
#11083=CARTESIAN_POINT('Ctrl Pts',(3.90000330864444,1.58823869807682,0.695355823328757));
#11084=CARTESIAN_POINT('Ctrl Pts',(3.90000209726118,1.58060840086481,0.697526456028474));
#11085=CARTESIAN_POINT('Ctrl Pts',(3.90000112250675,1.5728228815436,0.698773197673241));
#11086=CARTESIAN_POINT('Ctrl Pts',(3.90000049100668,1.56777898966077,0.699580906164169));
#11087=CARTESIAN_POINT('Ctrl Pts',(3.89999999374416,1.56266934880282,0.69999999924861));
#11088=CARTESIAN_POINT('Ctrl Pts',(3.89999999700315,1.55753217437,0.7));
#11089=CARTESIAN_POINT('Ctrl Pts',(3.9,1.68995649764597,0.));
#11090=CARTESIAN_POINT('Ctrl Pts',(3.9,1.68454744095908,0.101111134163871));
#11091=CARTESIAN_POINT('Ctrl Pts',(3.9,1.67913787721413,0.202223216861756));
#11092=CARTESIAN_POINT('Ctrl Pts',(3.9,1.66834172806373,0.404000675610066));
#11093=CARTESIAN_POINT('Ctrl Pts',(3.9,1.66295504272671,0.504667995047933));
#11094=CARTESIAN_POINT('Ctrl Pts',(3.9,1.657567947596,0.605334330700044));
#11095=CARTESIAN_POINT('Ctrl Pts',(3.90000000000029,-1.68995649764598,2.25514051876985E-17));
#11096=CARTESIAN_POINT('Ctrl Pts',(3.90375240214247,-1.67935614215062,0.202290156525516));
#11097=CARTESIAN_POINT('Ctrl Pts',(3.90750491350916,-1.66875579641967,0.404580311547879));
#11098=CARTESIAN_POINT('Ctrl Pts',(3.91125753584366,-1.65815546066147,0.606870465045848));
#11099=CARTESIAN_POINT('Ctrl Pts',(2.95719731373254,-1.63434162994996,-0.000186284957671625));
#11100=CARTESIAN_POINT('Ctrl Pts',(2.96263618266967,-1.62374249289717,0.202103577800055));
#11101=CARTESIAN_POINT('Ctrl Pts',(2.96807524459186,-1.6131433886527,0.404393433349269));
#11102=CARTESIAN_POINT('Ctrl Pts',(2.97351444051957,-1.60254429060724,0.606683290324339));
#11103=CARTESIAN_POINT('Ctrl Pts',(2.0151035222252,-1.5373601393942,-0.000515615972119944));
#11104=CARTESIAN_POINT('Ctrl Pts',(2.0222299762717,-1.52676329064944,0.20177372753372));
#11105=CARTESIAN_POINT('Ctrl Pts',(2.02935668076532,-1.51616649670304,0.404063061036967));
#11106=CARTESIAN_POINT('Ctrl Pts',(2.03648357820815,-1.50556972342972,0.606352393906678));
#11107=CARTESIAN_POINT('Ctrl Pts',(1.07355614839761,-1.3885225322474,-0.00102014041634142));
#11108=CARTESIAN_POINT('Ctrl Pts',(1.08237048982668,-1.37792954541675,0.201268457136957));
#11109=CARTESIAN_POINT('Ctrl Pts',(1.09118510562603,-1.36733662501784,0.403557046289628));
#11110=CARTESIAN_POINT('Ctrl Pts',(1.09999999998551,-1.35674377243019,0.605845626932519));
#11111=CARTESIAN_POINT('Ctrl Pts',(1.10000000359112,-1.35674374984279,0.605845627045242));
#11112=CARTESIAN_POINT('Ctrl Pts',(2.02777573897866,-1.50422778688462,0.60559460123127));
#11113=CARTESIAN_POINT('Ctrl Pts',(2.96295221054883,-1.60165319397541,0.605428415101273));
#11114=CARTESIAN_POINT('Ctrl Pts',(3.9,-1.657567947596,0.605334330700044));
#11115=CARTESIAN_POINT('Ctrl Pts',(3.90594750914669,-1.55788759822396,0.7));
#11116=CARTESIAN_POINT('Ctrl Pts',(2.96654482017732,-1.50183737247472,0.7));
#11117=CARTESIAN_POINT('Ctrl Pts',(2.02939151553635,-1.40396309164617,0.7));
#11118=CARTESIAN_POINT('Ctrl Pts',(1.1,-1.25565664448621,0.7));
#11119=CARTESIAN_POINT('Ctrl Pts',(3.90422602671531,-1.58673967158186,0.7));
#11120=CARTESIAN_POINT('Ctrl Pts',(2.9639697519154,-1.53062009474021,0.699999324449154));
#11121=CARTESIAN_POINT('Ctrl Pts',(2.02587169016863,-1.43262076012027,0.700001792708215));
#11122=CARTESIAN_POINT('Ctrl Pts',(1.09546090287069,-1.28410178925883,0.700000000000001));
#11123=CARTESIAN_POINT('Ctrl Pts',(3.90124198563808,-1.6367522482393,0.676652244116846));
#11124=CARTESIAN_POINT('Ctrl Pts',(2.95951584878018,-1.58051528054544,0.676683243227538));
#11125=CARTESIAN_POINT('Ctrl Pts',(2.01975879699698,-1.48229505764113,0.676737195552829));
#11126=CARTESIAN_POINT('Ctrl Pts',(1.08759175402576,-1.33341535796084,0.676819902351873));
#11127=CARTESIAN_POINT('Ctrl Pts',(3.90006887217438,-1.65641364884095,0.626981005337021));
#11128=CARTESIAN_POINT('Ctrl Pts',(2.95775794493813,-1.6001648299169,0.627061170854983));
#11129=CARTESIAN_POINT('Ctrl Pts',(2.01735267249256,-1.50192280897576,0.627202240820629));
#11130=CARTESIAN_POINT('Ctrl Pts',(1.08446813262788,-1.35299014570964,0.627416665943555));
#11131=CARTESIAN_POINT('Ctrl Pts',(3.9,-1.657567947596,0.605334330700044));
#11132=CARTESIAN_POINT('Ctrl Pts',(2.95765589353472,-1.60133715645388,0.605428946878649));
#11133=CARTESIAN_POINT('Ctrl Pts',(2.01720431860088,-1.50312513840151,0.605596482146283));
#11134=CARTESIAN_POINT('Ctrl Pts',(1.0842689834292,-1.35423815332579,0.605849891671036));
#11135=CARTESIAN_POINT('Ctrl Pts',(3.89999999700313,-1.55753217437,0.7));
#11136=CARTESIAN_POINT('Ctrl Pts',(2.96258932077475,-1.50142404037792,0.7));
#11137=CARTESIAN_POINT('Ctrl Pts',(2.02743012901897,-1.40365010593343,0.7));
#11138=CARTESIAN_POINT('Ctrl Pts',(1.1,-1.25565664448621,0.7));
#11139=CARTESIAN_POINT('Origin',(6.08012166120517,1.06778195214465E-16,
0.7));
#11140=CARTESIAN_POINT('Ctrl Pts',(1.1,1.25565664448621,0.7));
#11141=CARTESIAN_POINT('Ctrl Pts',(2.02743012901899,1.40365010593344,0.7));
#11142=CARTESIAN_POINT('Ctrl Pts',(2.96258932077472,1.50142404037792,0.7));
#11143=CARTESIAN_POINT('Ctrl Pts',(3.89999999700315,1.55753217437,0.7));
#11144=CARTESIAN_POINT('Ctrl Pts',(1.1,1.25565664448621,0.7));
#11145=CARTESIAN_POINT('Ctrl Pts',(2.02939151553637,1.40396309164617,0.7));
#11146=CARTESIAN_POINT('Ctrl Pts',(2.96654482017727,1.50183737247472,0.7));
#11147=CARTESIAN_POINT('Ctrl Pts',(3.90594750914669,1.55788759822396,0.7));
#11148=CARTESIAN_POINT('Ctrl Pts',(1.09546090287069,1.28410178925883,0.700000000000001));
#11149=CARTESIAN_POINT('Ctrl Pts',(2.02587169016866,1.43262076012027,0.700001792708215));
#11150=CARTESIAN_POINT('Ctrl Pts',(2.96396975191535,1.53062009474021,0.699999324449154));
#11151=CARTESIAN_POINT('Ctrl Pts',(3.90422602671531,1.58673967158186,0.7));
#11152=CARTESIAN_POINT('Ctrl Pts',(1.08759175402576,1.33341535796084,0.676819902351873));
#11153=CARTESIAN_POINT('Ctrl Pts',(2.019758796997,1.48229505764113,0.676737195552829));
#11154=CARTESIAN_POINT('Ctrl Pts',(2.95951584878014,1.58051528054544,0.676683243227538));
#11155=CARTESIAN_POINT('Ctrl Pts',(3.90124198563808,1.6367522482393,0.676652244116846));
#11156=CARTESIAN_POINT('Ctrl Pts',(1.08446813262788,1.35299014570964,0.627416665943555));
#11157=CARTESIAN_POINT('Ctrl Pts',(2.01735267249258,1.50192280897576,0.627202240820629));
#11158=CARTESIAN_POINT('Ctrl Pts',(2.95775794493809,1.6001648299169,0.627061170854983));
#11159=CARTESIAN_POINT('Ctrl Pts',(3.90006887217438,1.65641364884095,0.626981005337021));
#11160=CARTESIAN_POINT('Ctrl Pts',(1.0842689834292,1.35423815332579,0.605849891671036));
#11161=CARTESIAN_POINT('Ctrl Pts',(2.0172043186009,1.50312513840152,0.605596482146283));
#11162=CARTESIAN_POINT('Ctrl Pts',(2.95765589353468,1.60133715645387,0.605428946878649));
#11163=CARTESIAN_POINT('Ctrl Pts',(3.9,1.657567947596,0.605334330700044));
#11164=CARTESIAN_POINT('Ctrl Pts',(3.9,1.657567947596,0.605334330700044));
#11165=CARTESIAN_POINT('Ctrl Pts',(2.96295221054879,1.60165319397541,0.605428415101273));
#11166=CARTESIAN_POINT('Ctrl Pts',(2.02777573897867,1.50422778688462,0.60559460123127));
#11167=CARTESIAN_POINT('Ctrl Pts',(1.10000000359111,1.35674374984279,0.605845627045242));
#11168=CARTESIAN_POINT('Ctrl Pts',(1.07355614839761,1.3885225322474,-0.00102014041634139));
#11169=CARTESIAN_POINT('Ctrl Pts',(1.08237048982668,1.37792954541676,0.201268457136957));
#11170=CARTESIAN_POINT('Ctrl Pts',(1.09118510562602,1.36733662501784,0.403557046289628));
#11171=CARTESIAN_POINT('Ctrl Pts',(1.09999999998551,1.35674377243019,0.605845626932519));
#11172=CARTESIAN_POINT('Ctrl Pts',(2.0151035222252,1.5373601393942,-0.000515615972119942));
#11173=CARTESIAN_POINT('Ctrl Pts',(2.0222299762717,1.52676329064944,0.201773727533721));
#11174=CARTESIAN_POINT('Ctrl Pts',(2.02935668076532,1.51616649670304,0.404063061036968));
#11175=CARTESIAN_POINT('Ctrl Pts',(2.03648357820815,1.50556972342972,0.606352393906678));
#11176=CARTESIAN_POINT('Ctrl Pts',(2.95719731373254,1.63434162994996,-0.000186284957671606));
#11177=CARTESIAN_POINT('Ctrl Pts',(2.96263618266967,1.62374249289717,0.202103577800055));
#11178=CARTESIAN_POINT('Ctrl Pts',(2.96807524459186,1.6131433886527,0.404393433349269));
#11179=CARTESIAN_POINT('Ctrl Pts',(2.97351444051957,1.60254429060724,0.60668329032434));
#11180=CARTESIAN_POINT('Ctrl Pts',(3.90000000000029,1.68995649764598,4.33680868994202E-17));
#11181=CARTESIAN_POINT('Ctrl Pts',(3.90375240214247,1.67935614215062,0.202290156525516));
#11182=CARTESIAN_POINT('Ctrl Pts',(3.90750491350917,1.66875579641967,0.404580311547879));
#11183=CARTESIAN_POINT('Ctrl Pts',(3.91125753584366,1.65815546066147,0.606870465045848));
#11184=CARTESIAN_POINT('Origin',(0.9,1.44962962962963,0.));
#11185=CARTESIAN_POINT('',(0.900000000000025,-1.32415632515176,0.605901073595307));
#11186=CARTESIAN_POINT('Ctrl Pts',(0.900000000000025,-1.32415632515176,
0.605901073595307));
#11187=CARTESIAN_POINT('Ctrl Pts',(0.900000000000025,-1.33021622058432,
0.504787384877132));
#11188=CARTESIAN_POINT('Ctrl Pts',(0.900000000000001,-1.33627289299046,
0.403672458220672));
#11189=CARTESIAN_POINT('Ctrl Pts',(0.900000000000001,-1.3483639425303,0.201706128802639));
#11190=CARTESIAN_POINT('Ctrl Pts',(0.9,-1.3543984610184,0.100852646477479));
#11191=CARTESIAN_POINT('Ctrl Pts',(0.9,-1.3604297237941,0.));
#11192=CARTESIAN_POINT('',(0.9,-1.22294421121193,0.7));
#11193=CARTESIAN_POINT('Ctrl Pts',(0.899999998934589,-1.2229442093848,0.7));
#11194=CARTESIAN_POINT('Ctrl Pts',(0.89999998269596,-1.2309559991361,0.699999991698178));
#11195=CARTESIAN_POINT('Ctrl Pts',(0.900003161357076,-1.2389110096839,0.699008412490225));
#11196=CARTESIAN_POINT('Ctrl Pts',(0.900005837532895,-1.24666554379878,
0.697120920272419));
#11197=CARTESIAN_POINT('Ctrl Pts',(0.900007138246235,-1.25043451364619,
0.69620353424371));
#11198=CARTESIAN_POINT('Ctrl Pts',(0.900008321383585,-1.25415610217771,
0.695073675615989));
#11199=CARTESIAN_POINT('Ctrl Pts',(0.900009136546862,-1.25781268161099,
0.69373809091454));
#11200=CARTESIAN_POINT('Ctrl Pts',(0.90001081442992,-1.26533916477404,0.690989003700189));
#11201=CARTESIAN_POINT('Ctrl Pts',(0.900010659344479,-1.27251458345821,
0.687399440976464));
#11202=CARTESIAN_POINT('Ctrl Pts',(0.900008585023094,-1.27919110928202,
0.68304500924512));
#11203=CARTESIAN_POINT('Ctrl Pts',(0.900007251085311,-1.28348459539356,
0.680244796581297));
#11204=CARTESIAN_POINT('Ctrl Pts',(0.900005156998288,-1.28757155292352,
0.67712723751572));
#11205=CARTESIAN_POINT('Ctrl Pts',(0.900003422242992,-1.29140570811059,
0.673703384872626));
#11206=CARTESIAN_POINT('Ctrl Pts',(0.90000203719427,-1.29446694202502,0.670969741262059));
#11207=CARTESIAN_POINT('Ctrl Pts',(0.90000088611098,-1.29734878548314,0.668056850549005));
#11208=CARTESIAN_POINT('Ctrl Pts',(0.900000936626746,-1.30003070819003,
0.664973821719563));
#11209=CARTESIAN_POINT('Ctrl Pts',(0.90000103432908,-1.30521780373233,0.659010948495488));
#11210=CARTESIAN_POINT('Ctrl Pts',(0.900005119671874,-1.30966005175478,
0.652412896960716));
#11211=CARTESIAN_POINT('Ctrl Pts',(0.900006662646281,-1.31329014967729,
0.64534035177384));
#11212=CARTESIAN_POINT('Ctrl Pts',(0.900006837929091,-1.31370253096037,
0.644536906434065));
#11213=CARTESIAN_POINT('Ctrl Pts',(0.900006988901759,-1.3141043809937,0.64372731654354));
#11214=CARTESIAN_POINT('Ctrl Pts',(0.900007112770807,-1.31449556093743,
0.642911804846506));
#11215=CARTESIAN_POINT('Ctrl Pts',(0.900008198175579,-1.31792328224658,
0.635765868899185));
#11216=CARTESIAN_POINT('Ctrl Pts',(0.900006415208278,-1.32049402672979,
0.628253543462219));
#11217=CARTESIAN_POINT('Ctrl Pts',(0.900003664797616,-1.32215034643222,
0.620540220943237));
#11218=CARTESIAN_POINT('Ctrl Pts',(0.900001948338234,-1.32318401225236,
0.615726538031782));
#11219=CARTESIAN_POINT('Ctrl Pts',(0.900000000000001,-1.32386068836271,
0.610833984830158));
#11220=CARTESIAN_POINT('Ctrl Pts',(0.900000000000001,-1.32415632515176,
0.605901073595307));
#11221=CARTESIAN_POINT('',(0.9,1.22294421121193,0.7));
#11222=CARTESIAN_POINT('',(0.9,0.724814814814815,0.7));
#11223=CARTESIAN_POINT('',(0.900000000000027,1.32415632515176,0.605901073595307));
#11224=CARTESIAN_POINT('Ctrl Pts',(0.900000000000001,1.32415632515176,0.605901073595307));
#11225=CARTESIAN_POINT('Ctrl Pts',(0.900000000000001,1.32368299187747,0.613798977756921));
#11226=CARTESIAN_POINT('Ctrl Pts',(0.900004523569871,1.32223544152535,0.621596324701597));
#11227=CARTESIAN_POINT('Ctrl Pts',(0.900006356724635,1.31990036466821,0.629134362570908));
#11228=CARTESIAN_POINT('Ctrl Pts',(0.900007328861843,1.3186620540024,0.633131846706937));
#11229=CARTESIAN_POINT('Ctrl Pts',(0.900007702029268,1.31717322147439,0.637056437951431));
#11230=CARTESIAN_POINT('Ctrl Pts',(0.900007358328755,1.31544117393516,0.640882963165587));
#11231=CARTESIAN_POINT('Ctrl Pts',(0.900006707239278,1.31216006761937,0.648131745755711));
#11232=CARTESIAN_POINT('Ctrl Pts',(0.900003091243194,1.3080468004769,0.654946293188228));
#11233=CARTESIAN_POINT('Ctrl Pts',(0.900001489347898,1.30317324258861,0.661167512355852));
#11234=CARTESIAN_POINT('Ctrl Pts',(0.900001155878064,1.30215870403359,0.662462596327245));
#11235=CARTESIAN_POINT('Ctrl Pts',(0.90000093695446,1.30111105636563,0.663731893727214));
#11236=CARTESIAN_POINT('Ctrl Pts',(0.90000091848414,1.30003070515708,0.664973821721807));
#11237=CARTESIAN_POINT('Ctrl Pts',(0.90000089007412,1.29836896897911,0.666884086330845));
#11238=CARTESIAN_POINT('Ctrl Pts',(0.900001333486324,1.29662987445651,0.668729618924651));
#11239=CARTESIAN_POINT('Ctrl Pts',(0.900001997973453,1.2948182721625,0.670508241825176));
#11240=CARTESIAN_POINT('Ctrl Pts',(0.900004083621534,1.28913213515815,0.676090865298813));
#11241=CARTESIAN_POINT('Ctrl Pts',(0.900007925915178,1.28279871831387,0.680954424681199));
#11242=CARTESIAN_POINT('Ctrl Pts',(0.900009431597099,1.27598654051802,0.685053039288488));
#11243=CARTESIAN_POINT('Ctrl Pts',(0.900010426918848,1.2714833923965,0.687762403198649));
#11244=CARTESIAN_POINT('Ctrl Pts',(0.900010579450444,1.26676996242859,0.690136867340003));
#11245=CARTESIAN_POINT('Ctrl Pts',(0.900009885932263,1.26188774903006,0.692153145632694));
#11246=CARTESIAN_POINT('Ctrl Pts',(0.900008832351734,1.25447077696631,0.695216239878874));
#11247=CARTESIAN_POINT('Ctrl Pts',(0.900005746465811,1.24674633448708,0.697421320974322));
#11248=CARTESIAN_POINT('Ctrl Pts',(0.900003140090462,1.23886595492982,0.6987028844583));
#11249=CARTESIAN_POINT('Ctrl Pts',(0.900001403206082,1.23361448254879,0.699556916322089));
#11250=CARTESIAN_POINT('Ctrl Pts',(0.899999988093253,1.22829309040712,0.699999994457486));
#11251=CARTESIAN_POINT('Ctrl Pts',(0.899999998934588,1.2229442093848,0.7));
#11252=CARTESIAN_POINT('Ctrl Pts',(0.9,1.3604297237941,0.));
#11253=CARTESIAN_POINT('Ctrl Pts',(0.9,1.35439838926384,0.100853846331769));
#11254=CARTESIAN_POINT('Ctrl Pts',(0.9,1.34836379894337,0.201708528537181));
#11255=CARTESIAN_POINT('Ctrl Pts',(0.9,1.33627274925098,0.403674857922336));
#11256=CARTESIAN_POINT('Ctrl Pts',(0.900000000000027,1.33021614867672,0.504788584706939));
#11257=CARTESIAN_POINT('Ctrl Pts',(0.900000000000027,1.32415632515176,0.605901073595307));
#11258=CARTESIAN_POINT('Ctrl Pts',(0.900000000000001,-1.3604297237941,-1.73472347597681E-18));
#11259=CARTESIAN_POINT('Ctrl Pts',(0.909119345746934,-1.34984469470005,
0.202150401646216));
#11260=CARTESIAN_POINT('Ctrl Pts',(0.918238975454288,-1.33925973741039,
0.404300794324169));
#11261=CARTESIAN_POINT('Ctrl Pts',(0.92735889343571,-1.32867485341111,0.606451177918334));
#11262=CARTESIAN_POINT('Ctrl Pts',(0.693791632045388,-1.32642527651154,
-0.000115194085079675));
#11263=CARTESIAN_POINT('Ctrl Pts',(0.703280422539661,-1.31584113310577,
0.202035038813999));
#11264=CARTESIAN_POINT('Ctrl Pts',(0.712769508818954,-1.30525706820637,
0.404185262036053));
#11265=CARTESIAN_POINT('Ctrl Pts',(0.722258895242942,-1.29467308328318,
0.606335475483814));
#11266=CARTESIAN_POINT('Ctrl Pts',(0.487608314405001,-1.28990207050556,
-0.000238777108575344));
#11267=CARTESIAN_POINT('Ctrl Pts',(0.497466558273561,-1.27931888757273,
0.201911276725417));
#11268=CARTESIAN_POINT('Ctrl Pts',(0.507325109482935,-1.26873579028159,
0.404061320158324));
#11269=CARTESIAN_POINT('Ctrl Pts',(0.517183972542757,-1.25815278023897,
0.606211353085106));
#11270=CARTESIAN_POINT('Ctrl Pts',(0.281447431601629,-1.2507496025167,-0.000370926150909055));
#11271=CARTESIAN_POINT('Ctrl Pts',(0.291675125201343,-1.24016745708839,
0.201778938960696));
#11272=CARTESIAN_POINT('Ctrl Pts',(0.301903137322998,-1.2295854048496,0.403928792940867));
#11273=CARTESIAN_POINT('Ctrl Pts',(0.312131472716966,-1.21900344770756,
0.606078635650713));
#11274=CARTESIAN_POINT('',(0.313137632044026,-1.21919552599285,0.606079286803921));
#11275=CARTESIAN_POINT('Ctrl Pts',(0.28146619846596,-1.25073018526678,-6.36968776335234E-17));
#11276=CARTESIAN_POINT('Ctrl Pts',(0.292023490345879,-1.2402182973453,0.20202640462578));
#11277=CARTESIAN_POINT('Ctrl Pts',(0.302580635585432,-1.22970674279184,
0.404052833452346));
#11278=CARTESIAN_POINT('Ctrl Pts',(0.313137632044028,-1.21919552599286,
0.606079286803922));
#11279=CARTESIAN_POINT('Ctrl Pts',(0.313137632044026,-1.21919552599285,
0.606079286803921));
#11280=CARTESIAN_POINT('Ctrl Pts',(0.508347756773358,-1.25646926692181,
0.606016122348466));
#11281=CARTESIAN_POINT('Ctrl Pts',(0.703992099548353,-1.29143758865737,
0.605956720831638));
#11282=CARTESIAN_POINT('Ctrl Pts',(0.900000000000031,-1.32415632515176,
0.605901073595307));
#11283=CARTESIAN_POINT('Ctrl Pts',(0.916434425702686,-1.22569269236154,
0.7));
#11284=CARTESIAN_POINT('Ctrl Pts',(0.72117838049967,-1.193102781986,0.7));
#11285=CARTESIAN_POINT('Ctrl Pts',(0.526295996270969,-1.15827411715321,
0.7));
#11286=CARTESIAN_POINT('Ctrl Pts',(0.3318563713692,-1.12115139781564,0.7));
#11287=CARTESIAN_POINT('Ctrl Pts',(0.911693828447622,-1.25409504944868,
0.700000000000001));
#11288=CARTESIAN_POINT('Ctrl Pts',(0.716221724293519,-1.22145811194286,
0.699999606692487));
#11289=CARTESIAN_POINT('Ctrl Pts',(0.52112301919326,-1.18657973614434,0.700000445015345));
#11290=CARTESIAN_POINT('Ctrl Pts',(0.32646265058614,-1.14940237362229,0.699999999999999));
#11291=CARTESIAN_POINT('Ctrl Pts',(0.903473253113197,-1.30334701150065,
0.676847307332805));
#11292=CARTESIAN_POINT('Ctrl Pts',(0.707628846166824,-1.27063023858114,
0.676865462359186));
#11293=CARTESIAN_POINT('Ctrl Pts',(0.512149925983835,-1.23566412474798,
0.676884474751893));
#11294=CARTESIAN_POINT('Ctrl Pts',(0.317109102097966,-1.19839394783867,
0.676905055067496));
#11295=CARTESIAN_POINT('Ctrl Pts',(0.900209809599689,-1.32289929215588,
0.627459885485154));
#11296=CARTESIAN_POINT('Ctrl Pts',(0.704212910592823,-1.29017057588713,
0.627506965865002));
#11297=CARTESIAN_POINT('Ctrl Pts',(0.50858160780484,-1.25519230329596,0.627556915196293));
#11298=CARTESIAN_POINT('Ctrl Pts',(0.31338355686088,-1.21790743260971,0.627610331402299));
#11299=CARTESIAN_POINT('Ctrl Pts',(0.900000000000031,-1.32415632515176,
0.605901073595307));
#11300=CARTESIAN_POINT('Ctrl Pts',(0.703992099548353,-1.29143758865737,
0.605956720831638));
#11301=CARTESIAN_POINT('Ctrl Pts',(0.508347756773358,-1.25646926692181,
0.606016122348466));
#11302=CARTESIAN_POINT('Ctrl Pts',(0.313137632044026,-1.21919552599285,
0.606079286803921));
#11303=CARTESIAN_POINT('',(0.3318563713692,-1.12115139781563,0.7));
#11304=CARTESIAN_POINT('Origin',(0.331856371369202,-1.12115139781563,0.6));
#11305=CARTESIAN_POINT('Ctrl Pts',(0.899999998934586,-1.2229442093848,0.7));
#11306=CARTESIAN_POINT('Ctrl Pts',(0.71024282334811,-1.19114655107378,0.7));
#11307=CARTESIAN_POINT('Ctrl Pts',(0.520840466228891,-1.15723253876768,
0.7));
#11308=CARTESIAN_POINT('Ctrl Pts',(0.3318563713692,-1.12115139781564,0.7));
#11309=CARTESIAN_POINT('Origin',(6.08012166120517,1.06778195214465E-16,
0.7));
#11310=CARTESIAN_POINT('',(0.331856371369203,1.12115139781563,0.7));
#11311=CARTESIAN_POINT('',(0.3318563713692,-0.7,0.7));
#11312=CARTESIAN_POINT('Ctrl Pts',(0.331856371369202,1.12115139781564,0.7));
#11313=CARTESIAN_POINT('Ctrl Pts',(0.520840466228894,1.15723253876768,0.7));
#11314=CARTESIAN_POINT('Ctrl Pts',(0.710242823348114,1.19114655107378,0.7));
#11315=CARTESIAN_POINT('Ctrl Pts',(0.899999998934589,1.2229442093848,0.7));
#11316=CARTESIAN_POINT('Ctrl Pts',(0.281447431601628,1.2507496025167,-0.000370926150909064));
#11317=CARTESIAN_POINT('Ctrl Pts',(0.291675125201342,1.24016745708839,0.201778938960695));
#11318=CARTESIAN_POINT('Ctrl Pts',(0.301903137322998,1.2295854048496,0.403928792940867));
#11319=CARTESIAN_POINT('Ctrl Pts',(0.312131472716965,1.21900344770756,0.606078635650713));
#11320=CARTESIAN_POINT('Ctrl Pts',(0.487608314405001,1.28990207050556,-0.000238777108575355));
#11321=CARTESIAN_POINT('Ctrl Pts',(0.497466558273561,1.27931888757273,0.201911276725417));
#11322=CARTESIAN_POINT('Ctrl Pts',(0.507325109482935,1.26873579028159,0.404061320158324));
#11323=CARTESIAN_POINT('Ctrl Pts',(0.517183972542757,1.25815278023897,0.606211353085106));
#11324=CARTESIAN_POINT('Ctrl Pts',(0.693791632045388,1.32642527651154,-0.000115194085079627));
#11325=CARTESIAN_POINT('Ctrl Pts',(0.703280422539661,1.31584113310577,0.202035038813999));
#11326=CARTESIAN_POINT('Ctrl Pts',(0.712769508818955,1.30525706820637,0.404185262036054));
#11327=CARTESIAN_POINT('Ctrl Pts',(0.722258895242942,1.29467308328318,0.606335475483814));
#11328=CARTESIAN_POINT('Ctrl Pts',(0.900000000000002,1.3604297237941,4.33680868994202E-17));
#11329=CARTESIAN_POINT('Ctrl Pts',(0.909119345746935,1.34984469470005,0.202150401646216));
#11330=CARTESIAN_POINT('Ctrl Pts',(0.918238975454289,1.33925973741039,0.40430079432417));
#11331=CARTESIAN_POINT('Ctrl Pts',(0.927358893435711,1.32867485341111,0.606451177918334));
#11332=CARTESIAN_POINT('',(0.313137632044028,1.21919552599286,0.606079286803921));
#11333=CARTESIAN_POINT('Ctrl Pts',(0.900000000000026,1.32415632515176,0.605901073595307));
#11334=CARTESIAN_POINT('Ctrl Pts',(0.703992099548352,1.29143758865737,0.605956720831638));
#11335=CARTESIAN_POINT('Ctrl Pts',(0.508347756773358,1.25646926692181,0.606016122348466));
#11336=CARTESIAN_POINT('Ctrl Pts',(0.313137632044028,1.21919552599286,0.606079286803921));
#11337=CARTESIAN_POINT('Ctrl Pts',(0.313137632044028,1.21919552599286,0.606079286803922));
#11338=CARTESIAN_POINT('Ctrl Pts',(0.302580635585432,1.22970674279184,0.404052833452346));
#11339=CARTESIAN_POINT('Ctrl Pts',(0.29202349034588,1.2402182973453,0.20202640462578));
#11340=CARTESIAN_POINT('Ctrl Pts',(0.28146619846596,1.25073018526678,-6.5594231435373E-18));
#11341=CARTESIAN_POINT('Ctrl Pts',(0.331856371369202,1.12115139781564,0.7));
#11342=CARTESIAN_POINT('Ctrl Pts',(0.526295996270969,1.15827411715321,0.7));
#11343=CARTESIAN_POINT('Ctrl Pts',(0.72117838049967,1.193102781986,0.7));
#11344=CARTESIAN_POINT('Ctrl Pts',(0.916434425702682,1.22569269236154,0.7));
#11345=CARTESIAN_POINT('Ctrl Pts',(0.326462650586141,1.14940237362229,0.699999999999999));
#11346=CARTESIAN_POINT('Ctrl Pts',(0.52112301919326,1.18657973614434,0.700000445015345));
#11347=CARTESIAN_POINT('Ctrl Pts',(0.716221724293519,1.22145811194286,0.699999606692487));
#11348=CARTESIAN_POINT('Ctrl Pts',(0.911693828447618,1.25409504944868,0.700000000000001));
#11349=CARTESIAN_POINT('Ctrl Pts',(0.317109102097967,1.19839394783867,0.676905055067496));
#11350=CARTESIAN_POINT('Ctrl Pts',(0.512149925983836,1.23566412474798,0.676884474751893));
#11351=CARTESIAN_POINT('Ctrl Pts',(0.707628846166824,1.27063023858114,0.676865462359185));
#11352=CARTESIAN_POINT('Ctrl Pts',(0.903473253113193,1.30334701150065,0.676847307332805));
#11353=CARTESIAN_POINT('Ctrl Pts',(0.313383556860882,1.21790743260971,0.627610331402299));
#11354=CARTESIAN_POINT('Ctrl Pts',(0.508581607804839,1.25519230329596,0.627556915196293));
#11355=CARTESIAN_POINT('Ctrl Pts',(0.704212910592822,1.29017057588713,0.627506965865002));
#11356=CARTESIAN_POINT('Ctrl Pts',(0.900209809599685,1.32289929215587,0.627459885485154));
#11357=CARTESIAN_POINT('Ctrl Pts',(0.313137632044028,1.21919552599286,0.606079286803921));
#11358=CARTESIAN_POINT('Ctrl Pts',(0.508347756773358,1.25646926692181,0.606016122348466));
#11359=CARTESIAN_POINT('Ctrl Pts',(0.703992099548352,1.29143758865737,0.605956720831638));
#11360=CARTESIAN_POINT('Ctrl Pts',(0.900000000000026,1.32415632515176,0.605901073595307));
#11361=CARTESIAN_POINT('Origin',(0.3318563713692,1.12115139781563,0.6));
#11362=CARTESIAN_POINT('Origin',(0.3318563713692,1.12115139781563,0.6));
#11363=CARTESIAN_POINT('Origin',(0.3318563713692,1.12115139781563,0.6));
#11364=CARTESIAN_POINT('Origin',(0.331856371369201,1.12115139781563,0.6));
#11365=CARTESIAN_POINT('Origin',(11.6681436286308,1.2964346619681,0.6));
#11366=CARTESIAN_POINT('Origin',(11.6681436286308,1.2964346619681,0.6));
#11367=CARTESIAN_POINT('',(11.7680065821063,1.2964346619681,0.605233595624295));
#11368=CARTESIAN_POINT('Origin',(11.6681436286308,1.2964346619681,0.6));
#11369=CARTESIAN_POINT('Origin',(11.6681436286308,1.2964346619681,0.6));
#11370=CARTESIAN_POINT('Origin',(0.3318563713692,-1.12115139781563,0.6));
#11371=CARTESIAN_POINT('Origin',(0.3318563713692,-1.12115139781563,0.6));
#11372=CARTESIAN_POINT('Origin',(0.3318563713692,-1.12115139781563,0.6));
#11373=CARTESIAN_POINT('Origin',(0.3318563713692,-0.7,0.6));
#11374=CARTESIAN_POINT('Ctrl Pts',(0.281398851089427,-1.25079724300364,
-0.00128877254616805));
#11375=CARTESIAN_POINT('Ctrl Pts',(0.291978592719145,-1.24026300108396,
0.201167222825305));
#11376=CARTESIAN_POINT('Ctrl Pts',(0.302558187088771,-1.2297290939422,0.403623242499903));
#11377=CARTESIAN_POINT('Ctrl Pts',(0.313137632044028,-1.21919552599286,
0.606079286803922));
#11378=CARTESIAN_POINT('Ctrl Pts',(0.258825925396095,-1.24645021448495,
-0.000331836826913007));
#11379=CARTESIAN_POINT('Ctrl Pts',(0.269412087408768,-1.23590982471973,
0.202123507634926));
#11380=CARTESIAN_POINT('Ctrl Pts',(0.279998097240749,-1.22537010804418,
0.404578894752494));
#11381=CARTESIAN_POINT('Ctrl Pts',(0.290584031570127,-1.21483034200885,
0.60703428203898));
#11382=CARTESIAN_POINT('Ctrl Pts',(0.216858515231733,-1.22156435206688,
0.000573427186746937));
#11383=CARTESIAN_POINT('Ctrl Pts',(0.22746089442761,-1.21102065820065,0.20302778119957));
#11384=CARTESIAN_POINT('Ctrl Pts',(0.238063405890532,-1.20047706879609,
0.405482132943502));
#11385=CARTESIAN_POINT('Ctrl Pts',(0.248665715176951,-1.18993398276804,
0.607936521147589));
#11386=CARTESIAN_POINT('Ctrl Pts',(0.20022524016831,-1.1757120364715,-0.000939345874739115));
#11387=CARTESIAN_POINT('Ctrl Pts',(0.210835545796271,-1.16517845930889,
0.201515175954065));
#11388=CARTESIAN_POINT('Ctrl Pts',(0.221445511453644,-1.15464532122135,
0.403969738345816));
#11389=CARTESIAN_POINT('Ctrl Pts',(0.232055819885544,-1.1441124535127,0.606424296559432));
#11390=CARTESIAN_POINT('Ctrl Pts',(0.200162791320387,-1.15273540576203,
-0.00213094087794781));
#11391=CARTESIAN_POINT('Ctrl Pts',(0.210772999146098,-1.14220702337553,
0.200323884929633));
#11392=CARTESIAN_POINT('Ctrl Pts',(0.221383207999129,-1.13167901896849,
0.402778730339676));
#11393=CARTESIAN_POINT('Ctrl Pts',(0.231993417893744,-1.12115139781563,
0.605233595624295));
#11394=CARTESIAN_POINT('Origin',(11.6681436286308,-1.2964346619681,0.6));
#11395=CARTESIAN_POINT('',(11.7680065821063,-1.2964346619681,0.605233595624295));
#11396=CARTESIAN_POINT('Origin',(11.6681436286308,-1.2964346619681,0.6));
#11397=CARTESIAN_POINT('Origin',(11.6681436286308,-1.2964346619681,0.6));
#11398=CARTESIAN_POINT('Origin',(11.6681436286308,0.8,0.6));
#11399=CARTESIAN_POINT('',(11.7680065821063,0.8,0.605233595624295));
#11400=CARTESIAN_POINT('Ctrl Pts',(11.7998406965532,-1.32812796269332,-0.00219749346969486));
#11401=CARTESIAN_POINT('Ctrl Pts',(11.7892293257052,-1.31756329650235,0.200279524124498));
#11402=CARTESIAN_POINT('Ctrl Pts',(11.778617954226,-1.30699886176745,0.402756553762325));
#11403=CARTESIAN_POINT('Ctrl Pts',(11.7680065821063,-1.2964346619681,0.605233595624295));
#11404=CARTESIAN_POINT('Ctrl Pts',(11.7997644051931,-1.35610429277321,-0.000741767599518841));
#11405=CARTESIAN_POINT('Ctrl Pts',(11.7891529352516,-1.34553639595159,0.201735054786578));
#11406=CARTESIAN_POINT('Ctrl Pts',(11.7785417923834,-1.33496887357233,0.404211913913734));
#11407=CARTESIAN_POINT('Ctrl Pts',(11.7679303202531,-1.32440140973518,0.606688758469115));
#11408=CARTESIAN_POINT('Ctrl Pts',(11.777798894316,-1.40464673224301,0.000639873095493681));
#11409=CARTESIAN_POINT('Ctrl Pts',(11.7671928076068,-1.39407357725403,0.203116666245104));
#11410=CARTESIAN_POINT('Ctrl Pts',(11.7565866683578,-1.38350056680667,0.405593463707878));
#11411=CARTESIAN_POINT('Ctrl Pts',(11.7459806329718,-1.37292778989405,0.608070278434593));
#11412=CARTESIAN_POINT('Ctrl Pts',(11.7305637688674,-1.42539741767755,-0.000752904078362463));
#11413=CARTESIAN_POINT('Ctrl Pts',(11.7199663219939,-1.4148278080644,0.201724510929383));
#11414=CARTESIAN_POINT('Ctrl Pts',(11.7093688723049,-1.40425849106451,0.404201940657439));
#11415=CARTESIAN_POINT('Ctrl Pts',(11.6987715660822,-1.39368929079062,0.606679383299034));
#11416=CARTESIAN_POINT('Ctrl Pts',(11.7096810564041,-1.4274931182575,-0.0017379730583696));
#11417=CARTESIAN_POINT('Ctrl Pts',(11.6990862989954,-1.41692678914967,0.200739752511227));
#11418=CARTESIAN_POINT('Ctrl Pts',(11.6884916259906,-1.40636067879325,0.403217493356832));
#11419=CARTESIAN_POINT('Ctrl Pts',(11.6778970386953,-1.39579479040469,0.605695249702977));
#11420=CARTESIAN_POINT('Ctrl Pts',(11.7997255308004,-1.32801330383774,1.58293517182884E-17));
#11421=CARTESIAN_POINT('Ctrl Pts',(11.7891525485321,-1.31748685893698,0.201744519857947));
#11422=CARTESIAN_POINT('Ctrl Pts',(11.7785795656372,-1.30696064383315,0.403489051673192));
#11423=CARTESIAN_POINT('Ctrl Pts',(11.7680065821063,-1.2964346619681,0.605233595624295));
#11424=CARTESIAN_POINT('Ctrl Pts',(11.7096782931395,1.42749036240749,-0.00168516396645821));
#11425=CARTESIAN_POINT('Ctrl Pts',(11.6990844568337,1.41692495195436,0.200774958575157));
#11426=CARTESIAN_POINT('Ctrl Pts',(11.6884907049172,1.40635976021489,0.403235096390144));
#11427=CARTESIAN_POINT('Ctrl Pts',(11.6778970386953,1.39579479040469,0.605695249702978));
#11428=CARTESIAN_POINT('Ctrl Pts',(11.7375219088137,1.42469609383707,-0.000371738767665111));
#11429=CARTESIAN_POINT('Ctrl Pts',(11.7269244310859,1.41412622652679,0.202087962343291));
#11430=CARTESIAN_POINT('Ctrl Pts',(11.7163270893473,1.40355692684423,0.404547700208143));
#11431=CARTESIAN_POINT('Ctrl Pts',(11.7057297418778,1.39298745758592,0.607007427831054));
#11432=CARTESIAN_POINT('Ctrl Pts',(11.7837126264455,1.39812338730171,0.000662527065309348));
#11433=CARTESIAN_POINT('Ctrl Pts',(11.7731059659782,1.38755170250994,0.203121672627585));
#11434=CARTESIAN_POINT('Ctrl Pts',(11.762499302106,1.37698011891703,0.405580822779681));
#11435=CARTESIAN_POINT('Ctrl Pts',(11.7518926781287,1.36640881816393,0.608039989525598));
#11436=CARTESIAN_POINT('Ctrl Pts',(11.7997807104374,1.34910745421534,-0.00105289019631603));
#11437=CARTESIAN_POINT('Ctrl Pts',(11.7891702365097,1.33854134055748,0.201406383632416));
#11438=CARTESIAN_POINT('Ctrl Pts',(11.7785598611315,1.32797539467558,0.403865671186622));
#11439=CARTESIAN_POINT('Ctrl Pts',(11.7679493857164,1.31740972279341,0.60632496775791));
#11440=CARTESIAN_POINT('Ctrl Pts',(11.7998379289556,1.32812520727701,-0.00214468456243374));
#11441=CARTESIAN_POINT('Ctrl Pts',(11.78922748064,1.31756145959839,0.200314730064766));
#11442=CARTESIAN_POINT('Ctrl Pts',(11.7786170316934,1.30699794333589,0.402774156733522));
#11443=CARTESIAN_POINT('Ctrl Pts',(11.7680065821063,1.2964346619681,0.605233595624295));
#11444=CARTESIAN_POINT('Ctrl Pts',(11.7680065821063,1.2964346619681,0.605233595624295));
#11445=CARTESIAN_POINT('Ctrl Pts',(11.7785795656372,1.30696064383315,0.403489051673192));
#11446=CARTESIAN_POINT('Ctrl Pts',(11.7891525485321,1.31748685893698,0.201744519857946));
#11447=CARTESIAN_POINT('Ctrl Pts',(11.7997255308004,1.32801330383774,3.10081821330854E-17));
#11448=CARTESIAN_POINT('Ctrl Pts',(11.3905090053564,1.32332268868375,0.7));
#11449=CARTESIAN_POINT('Ctrl Pts',(11.4830653488871,1.31448403714216,0.7));
#11450=CARTESIAN_POINT('Ctrl Pts',(11.5756099286391,1.3055179747114,0.7));
#11451=CARTESIAN_POINT('Ctrl Pts',(11.6681436286308,1.2964346619681,0.7));
#11452=CARTESIAN_POINT('Ctrl Pts',(11.3932507170007,1.35203326785047,0.7));
#11453=CARTESIAN_POINT('Ctrl Pts',(11.4858332859074,1.34318985044544,0.699999917777441));
#11454=CARTESIAN_POINT('Ctrl Pts',(11.5784027531871,1.33421922733773,0.700000082825348));
#11455=CARTESIAN_POINT('Ctrl Pts',(11.6709605510772,1.32513126902304,0.7));
#11456=CARTESIAN_POINT('Ctrl Pts',(11.3980029235658,1.40179729139028,0.67675176769038));
#11457=CARTESIAN_POINT('Ctrl Pts',(11.4906306781252,1.39294591144353,0.676755553516685));
#11458=CARTESIAN_POINT('Ctrl Pts',(11.583243842395,1.38396722707511,0.676759299309383));
#11459=CARTESIAN_POINT('Ctrl Pts',(11.6758431636759,1.37487151491717,0.676763114282959));
#11460=CARTESIAN_POINT('Ctrl Pts',(11.3998836071583,1.4214913811319,0.627256563056779));
#11461=CARTESIAN_POINT('Ctrl Pts',(11.4925297866457,1.41264104586547,0.627266369072496));
#11462=CARTESIAN_POINT('Ctrl Pts',(11.5851604051362,1.40366358810601,0.627276165220861));
#11463=CARTESIAN_POINT('Ctrl Pts',(11.6777767156198,1.39456903283364,0.627286048421068));
#11464=CARTESIAN_POINT('Ctrl Pts',(11.4,1.4227102204299,0.605660349289938));
#11465=CARTESIAN_POINT('Ctrl Pts',(11.4926474653491,1.41386220753305,0.605671932550561));
#11466=CARTESIAN_POINT('Ctrl Pts',(11.585279512325,1.40488700096013,0.605683574233495));
#11467=CARTESIAN_POINT('Ctrl Pts',(11.6778970386953,1.39579479040469,0.605695249702977));
#11468=CARTESIAN_POINT('Ctrl Pts',(0.200160078391861,1.15273809776858,-0.00218270663797729));
#11469=CARTESIAN_POINT('Ctrl Pts',(0.210771190526905,1.14220881798213,0.200289374419605));
#11470=CARTESIAN_POINT('Ctrl Pts',(0.221382303689445,1.13167991623912,0.402761475082968));
#11471=CARTESIAN_POINT('Ctrl Pts',(0.231993417893744,1.12115139781563,0.605233595624295));
#11472=CARTESIAN_POINT('Ctrl Pts',(0.200222527243758,1.17571472979894,-0.000991111558954063));
#11473=CARTESIAN_POINT('Ctrl Pts',(0.210833737189325,1.165180254798,0.201480665494204));
#11474=CARTESIAN_POINT('Ctrl Pts',(0.22144460713556,1.15464621893915,0.403952483115279));
#11475=CARTESIAN_POINT('Ctrl Pts',(0.232055819885544,1.1441124535127,0.606424296559433));
#11476=CARTESIAN_POINT('Ctrl Pts',(0.216855804290742,1.22156704800519,0.000521661548984882));
#11477=CARTESIAN_POINT('Ctrl Pts',(0.22745908713481,1.21102245544698,0.202993270772045));
#11478=CARTESIAN_POINT('Ctrl Pts',(0.238062502254218,1.2004779673848,0.405464877727456));
#11479=CARTESIAN_POINT('Ctrl Pts',(0.248665715176951,1.18993398276804,0.607936521147589));
#11480=CARTESIAN_POINT('Ctrl Pts',(0.258823218619159,1.24645290953083,-0.000383602721372307));
#11481=CARTESIAN_POINT('Ctrl Pts',(0.269410282911183,1.23591162135389,0.202088997034388));
#11482=CARTESIAN_POINT('Ctrl Pts',(0.279997195000074,1.22537100634993,0.404561639451295));
#11483=CARTESIAN_POINT('Ctrl Pts',(0.290584031570127,1.21483034200885,0.60703428203898));
#11484=CARTESIAN_POINT('Ctrl Pts',(0.281396145950812,1.25079993650842,-0.00134053860524368));
#11485=CARTESIAN_POINT('Ctrl Pts',(0.291976789318506,1.24026479669674,0.201132712115111));
#11486=CARTESIAN_POINT('Ctrl Pts',(0.302557285401186,1.22972999171968,0.403605987142707));
#11487=CARTESIAN_POINT('Ctrl Pts',(0.313137632044028,1.21919552599286,0.606079286803922));
#11488=CARTESIAN_POINT('Origin',(11.8002740930491,1.6,-0.0104671912485888));
#11489=CARTESIAN_POINT('Origin',(0.3318563713692,1.12115139781563,0.6));
#11490=CARTESIAN_POINT('',(0.331856371369203,1.12115139781563,0.9));
#11491=CARTESIAN_POINT('',(0.0322675109428288,1.12115139781563,0.615700786872883));
#11492=CARTESIAN_POINT('Origin',(0.3318563713692,1.12115139781563,0.6));
#11493=CARTESIAN_POINT('',(0.275700153393682,1.4152837823473,0.618237860411764));
#11494=CARTESIAN_POINT('Origin',(0.3318563713692,1.12115139781563,0.6));
#11495=CARTESIAN_POINT('Origin',(0.331856371369201,1.12115139781563,0.600000000000001));
#11496=CARTESIAN_POINT('Origin',(11.6681436286308,1.2964346619681,0.6));
#11497=CARTESIAN_POINT('',(11.6681436286308,1.2964346619681,0.9));
#11498=CARTESIAN_POINT('',(11.6974038588243,1.59451504727786,0.617085749108931));
#11499=CARTESIAN_POINT('Origin',(11.6681436286308,1.2964346619681,0.6));
#11500=CARTESIAN_POINT('',(11.9677324890572,1.2964346619681,0.615700786872884));
#11501=CARTESIAN_POINT('Origin',(11.6681436286308,1.2964346619681,0.6));
#11502=CARTESIAN_POINT('Origin',(11.6681436286308,1.2964346619681,0.6));
#11503=CARTESIAN_POINT('Origin',(0.3318563713692,-1.12115139781563,0.6));
#11504=CARTESIAN_POINT('',(0.3318563713692,-1.12115139781563,0.9));
#11505=CARTESIAN_POINT('',(0.27570015339368,-1.4152837823473,0.618237860411764));
#11506=CARTESIAN_POINT('Origin',(0.331856371369206,-1.12115139781563,0.6));
#11507=CARTESIAN_POINT('',(0.0322675109428289,-1.12115139781563,0.615700786872884));
#11508=CARTESIAN_POINT('Origin',(0.3318563713692,-1.12115139781563,0.6));
#11509=CARTESIAN_POINT('Origin',(0.331856371369201,-1.12115139781563,0.6));
#11510=CARTESIAN_POINT('Origin',(0.3318563713692,-0.7,0.6));
#11511=CARTESIAN_POINT('',(0.0322675109428288,-0.7,0.615700786872883));
#11512=CARTESIAN_POINT('',(0.3318563713692,-0.7,0.9));
#11513=CARTESIAN_POINT('Ctrl Pts',(0.243379792658812,-1.44768816351885,
-0.00386660544379547));
#11514=CARTESIAN_POINT('Ctrl Pts',(0.254153714020244,-1.43688644166428,
0.203501514337738));
#11515=CARTESIAN_POINT('Ctrl Pts',(0.264927169923045,-1.42608498030896,
0.410869669467268));
#11516=CARTESIAN_POINT('Ctrl Pts',(0.275700153393682,-1.4152837823473,0.618237860411764));
#11517=CARTESIAN_POINT('Ctrl Pts',(0.165985306518657,-1.43278556900406,
-0.000585522405354874));
#11518=CARTESIAN_POINT('Ctrl Pts',(0.176781886982148,-1.42196211044871,
0.206780297826791));
#11519=CARTESIAN_POINT('Ctrl Pts',(0.187577631459021,-1.41114055376332,
0.414146260476818));
#11520=CARTESIAN_POINT('Ctrl Pts',(0.198373523197449,-1.40031743725927,
0.621512129789107));
#11521=CARTESIAN_POINT('Ctrl Pts',(0.0420337764471552,-1.35067831466576,
0.00164062070145552));
#11522=CARTESIAN_POINT('Ctrl Pts',(0.0528811856485653,-1.33984924001505,
0.209003590924217));
#11523=CARTESIAN_POINT('Ctrl Pts',(0.0637288270387668,-1.3290196870647,
0.416366521726085));
#11524=CARTESIAN_POINT('Ctrl Pts',(0.0745760486629849,-1.31819094697801,
0.623729515932473));
#11525=CARTESIAN_POINT('Ctrl Pts',(-0.000174449685670057,-1.21258510413485,
-0.00332869829739982));
#11526=CARTESIAN_POINT('Ctrl Pts',(0.0106931634330696,-1.20178787588112,
0.204035045544629));
#11527=CARTESIAN_POINT('Ctrl Pts',(0.0215603573327632,-1.19099068058357,
0.411398812224037));
#11528=CARTESIAN_POINT('Ctrl Pts',(0.0324279732074593,-1.18019411246525,
0.618762589277523));
#11529=CARTESIAN_POINT('Ctrl Pts',(-0.000335035344191381,-1.15350137313465,
-0.00639285519773308));
#11530=CARTESIAN_POINT('Ctrl Pts',(0.0105324790023165,-1.1427176497384,
0.200971671503832));
#11531=CARTESIAN_POINT('Ctrl Pts',(0.0213999944262164,-1.13193432274319,
0.408336218763261));
#11532=CARTESIAN_POINT('Ctrl Pts',(0.0322675109428286,-1.12115139781563,
0.615700786872884));
#11533=CARTESIAN_POINT('Ctrl Pts',(0.243580684154575,-1.44748675362873,
-2.16840434497101E-17));
#11534=CARTESIAN_POINT('Ctrl Pts',(0.254287635915809,-1.43675217163244,
0.206079251738322));
#11535=CARTESIAN_POINT('Ctrl Pts',(0.264994127943615,-1.42601784692504,
0.412158538389471));
#11536=CARTESIAN_POINT('Ctrl Pts',(0.275700153393682,-1.4152837823473,0.618237860411764));
#11537=CARTESIAN_POINT('Ctrl Pts',(0.0322675109428286,-1.12115139781563,
0.615700786872884));
#11538=CARTESIAN_POINT('Ctrl Pts',(0.0215116728964671,-1.13182351356624,
0.410467170919192));
#11539=CARTESIAN_POINT('Ctrl Pts',(0.0107558359204751,-1.14249602316337,
0.205233575389367));
#11540=CARTESIAN_POINT('Ctrl Pts',(-1.41190227911925E-16,-1.15316892111333,
8.06646416329215E-17));
#11541=CARTESIAN_POINT('Origin',(11.6681436286308,-1.2964346619681,0.6));
#11542=CARTESIAN_POINT('',(11.9677324890572,-1.2964346619681,0.615700786872884));
#11543=CARTESIAN_POINT('',(11.6974038588243,-1.59451504727786,0.617085749108931));
#11544=CARTESIAN_POINT('Origin',(11.6681436286308,-1.2964346619681,0.600000000000001));
#11545=CARTESIAN_POINT('',(11.6681436286308,-1.2964346619681,0.9));
#11546=CARTESIAN_POINT('Origin',(11.6681436286308,-1.2964346619681,0.6));
#11547=CARTESIAN_POINT('Origin',(11.6681436286308,-1.2964346619681,0.6));
#11548=CARTESIAN_POINT('Origin',(11.6681436286308,0.8,0.6));
#11549=CARTESIAN_POINT('',(11.9677324890572,0.8,0.615700786872884));
#11550=CARTESIAN_POINT('',(11.6681436286308,0.8,0.9));
#11551=CARTESIAN_POINT('Ctrl Pts',(11.6681436286308,-1.2964346619681,0.9));
#11552=CARTESIAN_POINT('Ctrl Pts',(10.0505146497799,-1.45522470190849,0.9));
#11553=CARTESIAN_POINT('Ctrl Pts',(7.34698379851713,-1.66064017564263,0.9));
#11554=CARTESIAN_POINT('Ctrl Pts',(3.5507249968367,-1.5921338472202,0.9));
#11555=CARTESIAN_POINT('Ctrl Pts',(1.39628032950236,-1.32437289587156,0.9));
#11556=CARTESIAN_POINT('Ctrl Pts',(0.331856371369199,-1.12115139781563,
0.9));
#11557=CARTESIAN_POINT('Ctrl Pts',(11.6765943959699,-1.38252448313292,0.9));
#11558=CARTESIAN_POINT('Ctrl Pts',(10.0577014803155,-1.54155822929668,0.900004386952174));
#11559=CARTESIAN_POINT('Ctrl Pts',(7.35045927226653,-1.74750661992774,0.90000020513805));
#11560=CARTESIAN_POINT('Ctrl Pts',(3.54497585078588,-1.67885197560093,0.899998846478116));
#11561=CARTESIAN_POINT('Ctrl Pts',(1.38372480803625,-1.41002339692611,0.900007381454799));
#11562=CARTESIAN_POINT('Ctrl Pts',(0.315675209020016,-1.2059043252356,0.9));
#11563=CARTESIAN_POINT('Ctrl Pts',(11.6912432102654,-1.53175516862908,0.830242007927396));
#11564=CARTESIAN_POINT('Ctrl Pts',(10.070172518288,-1.69119563674726,0.830042231904815));
#11565=CARTESIAN_POINT('Ctrl Pts',(7.35645297288469,-1.89806162871739,0.829725685238203));
#11566=CARTESIAN_POINT('Ctrl Pts',(3.53503777381493,-1.8291593714544,0.829829026055289));
#11567=CARTESIAN_POINT('Ctrl Pts',(1.36192166831068,-1.55847530615989,0.830279056498203));
#11568=CARTESIAN_POINT('Ctrl Pts',(0.28762358730286,-1.35283178372728,0.830616544072481));
#11569=CARTESIAN_POINT('Ctrl Pts',(11.6970428895979,-1.59083777456472,0.681858145263203));
#11570=CARTESIAN_POINT('Ctrl Pts',(10.0750816081461,-1.75021732245097,0.681339641080976));
#11571=CARTESIAN_POINT('Ctrl Pts',(7.3588078744758,-1.95708146899443,0.680519979048775));
#11572=CARTESIAN_POINT('Ctrl Pts',(3.53113644431293,-1.88819699008302,0.68078748362792));
#11573=CARTESIAN_POINT('Ctrl Pts',(1.35331700817769,-1.61730376958615,0.681953432622034));
#11574=CARTESIAN_POINT('Ctrl Pts',(0.276437927844241,-1.41141950219787,
0.682830994206899));
#11575=CARTESIAN_POINT('Ctrl Pts',(11.6974038588243,-1.59451504727786,0.617085749108931));
#11576=CARTESIAN_POINT('Ctrl Pts',(10.0753786444688,-1.75377172884558,0.616473434532366));
#11577=CARTESIAN_POINT('Ctrl Pts',(7.35893161235257,-1.96044797105896,0.61550283428964));
#11578=CARTESIAN_POINT('Ctrl Pts',(3.53092277948893,-1.89162724517065,0.615818637525046));
#11579=CARTESIAN_POINT('Ctrl Pts',(1.35277799022997,-1.62098550016515,0.617200513836093));
#11580=CARTESIAN_POINT('Ctrl Pts',(0.27570015339368,-1.4152837823473,0.618237860411764));
#11581=CARTESIAN_POINT('Ctrl Pts',(0.27570015339368,-1.4152837823473,0.618237860411764));
#11582=CARTESIAN_POINT('Ctrl Pts',(1.35277799022997,-1.62098550016515,0.617200513836093));
#11583=CARTESIAN_POINT('Ctrl Pts',(3.53092277948893,-1.89162724517065,0.615818637525046));
#11584=CARTESIAN_POINT('Ctrl Pts',(7.35893161235257,-1.96044797105896,0.61550283428964));
#11585=CARTESIAN_POINT('Ctrl Pts',(10.0753786444688,-1.75377172884558,0.616473434532366));
#11586=CARTESIAN_POINT('Ctrl Pts',(11.6974038588243,-1.59451504727786,0.617085749108931));
#11587=CARTESIAN_POINT('Ctrl Pts',(11.6681436286308,-1.2964346619681,0.9));
#11588=CARTESIAN_POINT('Ctrl Pts',(10.0505146497799,-1.45522470190849,0.9));
#11589=CARTESIAN_POINT('Ctrl Pts',(7.34698379851713,-1.66064017564263,0.9));
#11590=CARTESIAN_POINT('Ctrl Pts',(3.5507249968367,-1.5921338472202,0.9));
#11591=CARTESIAN_POINT('Ctrl Pts',(1.39628032950236,-1.32437289587156,0.9));
#11592=CARTESIAN_POINT('Ctrl Pts',(0.331856371369199,-1.12115139781563,
0.9));
#11593=CARTESIAN_POINT('Ctrl Pts',(12.0003454972153,-1.32890342861544,-0.00659247958978532));
#11594=CARTESIAN_POINT('Ctrl Pts',(11.9894744951615,-1.31808026232082,0.200838596530835));
#11595=CARTESIAN_POINT('Ctrl Pts',(11.9786034924455,-1.30725733885828,0.408269685287046));
#11596=CARTESIAN_POINT('Ctrl Pts',(11.9677324890572,-1.2964346619681,0.615700786872884));
#11597=CARTESIAN_POINT('Ctrl Pts',(12.000116620981,-1.41283311850955,-0.00222526087931226));
#11598=CARTESIAN_POINT('Ctrl Pts',(11.9892453109784,-1.40200002127642,0.205205215027088));
#11599=CARTESIAN_POINT('Ctrl Pts',(11.9783750177566,-1.39116761830557,0.412635780645844));
#11600=CARTESIAN_POINT('Ctrl Pts',(11.9675037034976,-1.38033490526933,0.620066275407343));
#11601=CARTESIAN_POINT('Ctrl Pts',(11.9341774721098,-1.5584705948029,0.00191796595980313));
#11602=CARTESIAN_POINT('Ctrl Pts',(11.9233226835938,-1.54762133657986,0.209348350794306));
#11603=CARTESIAN_POINT('Ctrl Pts',(11.9124678718222,-1.53677206634062,0.416778732304926));
#11604=CARTESIAN_POINT('Ctrl Pts',(11.9016132473252,-1.52592301942363,0.624209134118803));
#11605=CARTESIAN_POINT('Ctrl Pts',(11.7925116537096,-1.62071287545028,-0.0022587989925734));
#11606=CARTESIAN_POINT('Ctrl Pts',(11.7816834491585,-1.6098745265243,0.205173499361722));
#11607=CARTESIAN_POINT('Ctrl Pts',(11.7708551999607,-1.59903658749835,0.41260581547062));
#11608=CARTESIAN_POINT('Ctrl Pts',(11.760027440985,-1.58819854843564,0.620038149897102));
#11609=CARTESIAN_POINT('Ctrl Pts',(11.7298629188572,-1.62699926142283,-0.0052140742384003));
#11610=CARTESIAN_POINT('Ctrl Pts',(11.7190429637906,-1.61617098622686,0.202219177289036));
#11611=CARTESIAN_POINT('Ctrl Pts',(11.708223275703,-1.60534291388117,0.409652451626141));
#11612=CARTESIAN_POINT('Ctrl Pts',(11.6974038588243,-1.59451504727786,0.617085749108931));
#11613=CARTESIAN_POINT('Ctrl Pts',(12.,-1.32855945177638,-1.94722710178397E-16));
#11614=CARTESIAN_POINT('Ctrl Pts',(11.9892441636707,-1.31785094954632,0.205233583190348));
#11615=CARTESIAN_POINT('Ctrl Pts',(11.978488326693,-1.30714268506935,0.410467178751997));
#11616=CARTESIAN_POINT('Ctrl Pts',(11.9677324890572,-1.2964346619681,0.615700786872884));
#11617=CARTESIAN_POINT('Ctrl Pts',(11.6974038588243,-1.59451504727786,0.617085749108931));
#11618=CARTESIAN_POINT('Ctrl Pts',(11.7081326228587,-1.605252190239,0.41139047675572));
#11619=CARTESIAN_POINT('Ctrl Pts',(11.7188616535763,-1.61598953550924,0.205695227161956));
#11620=CARTESIAN_POINT('Ctrl Pts',(11.7295909468525,-1.62672708026858,8.73866951023317E-17));
#11621=CARTESIAN_POINT('Ctrl Pts',(11.7298546566854,1.62699099289774,-0.00505567716946009));
#11622=CARTESIAN_POINT('Ctrl Pts',(11.719037455812,1.61616547398006,0.202324775346606));
#11623=CARTESIAN_POINT('Ctrl Pts',(11.7082205217827,1.60534015781013,0.409705250660816));
#11624=CARTESIAN_POINT('Ctrl Pts',(11.6974038588243,1.59451504727786,0.617085749108931));
#11625=CARTESIAN_POINT('Ctrl Pts',(11.8133862946664,1.61860913476435,-0.00111531114554236));
#11626=CARTESIAN_POINT('Ctrl Pts',(11.8025579038448,1.6077699189899,0.206263846261978));
#11627=CARTESIAN_POINT('Ctrl Pts',(11.7917299466398,1.59693199028804,0.41364309356145));
#11628=CARTESIAN_POINT('Ctrl Pts',(11.7809019683719,1.58609304882157,0.621022283493159));
#11629=CARTESIAN_POINT('Ctrl Pts',(11.9519653779615,1.53884931758497,0.00198566945999789));
#11630=CARTESIAN_POINT('Ctrl Pts',(11.9411087765487,1.52800449744246,0.209363119024413));
#11631=CARTESIAN_POINT('Ctrl Pts',(11.9302521502216,1.51715965702667,0.416740564833343));
#11632=CARTESIAN_POINT('Ctrl Pts',(11.9193956662674,1.50631506689811,0.624118030142866));
#11633=CARTESIAN_POINT('Ctrl Pts',(12.0001655389052,1.39184242582033,-0.00315867047762133));
#11634=CARTESIAN_POINT('Ctrl Pts',(11.9892972278067,1.38101476165208,0.204219175612729));
#11635=CARTESIAN_POINT('Ctrl Pts',(11.9784292129672,1.37018709651964,0.41159703650799));
#11636=CARTESIAN_POINT('Ctrl Pts',(11.9675608998875,1.35935984444403,0.618974903273729));
#11637=CARTESIAN_POINT('Ctrl Pts',(12.0003371960637,1.32889516399154,-0.00643408418199817));
#11638=CARTESIAN_POINT('Ctrl Pts',(11.9894689610601,1.31807475269516,0.200944193475792));
#11639=CARTESIAN_POINT('Ctrl Pts',(11.9786007253947,1.3072545841082,0.408322483762789));
#11640=CARTESIAN_POINT('Ctrl Pts',(11.9677324890572,1.2964346619681,0.615700786872884));
#11641=CARTESIAN_POINT('Ctrl Pts',(11.7295909468525,1.62672708026857,-8.50014503228635E-17));
#11642=CARTESIAN_POINT('Ctrl Pts',(11.7188616535763,1.61598953550924,0.205695227161956));
#11643=CARTESIAN_POINT('Ctrl Pts',(11.7081326228587,1.605252190239,0.411390476755719));
#11644=CARTESIAN_POINT('Ctrl Pts',(11.6974038588243,1.59451504727786,0.617085749108931));
#11645=CARTESIAN_POINT('Ctrl Pts',(11.9677324890572,1.2964346619681,0.615700786872884));
#11646=CARTESIAN_POINT('Ctrl Pts',(11.978488326693,1.30714268506935,0.410467178751997));
#11647=CARTESIAN_POINT('Ctrl Pts',(11.9892441636707,1.31785094954633,0.205233583190349));
#11648=CARTESIAN_POINT('Ctrl Pts',(12.,1.32855945177638,-2.38524477946811E-17));
#11649=CARTESIAN_POINT('Ctrl Pts',(0.3318563713692,1.12115139781563,0.9));
#11650=CARTESIAN_POINT('Ctrl Pts',(1.92849230856897,1.42598364489954,0.9));
#11651=CARTESIAN_POINT('Ctrl Pts',(5.71993880054687,1.76935652211139,0.9));
#11652=CARTESIAN_POINT('Ctrl Pts',(9.51130499016288,1.50815471522196,0.9));
#11653=CARTESIAN_POINT('Ctrl Pts',(11.6681436286308,1.2964346619681,0.9));
#11654=CARTESIAN_POINT('Ctrl Pts',(0.315675209020018,1.2059043252356,0.9));
#11655=CARTESIAN_POINT('Ctrl Pts',(1.91774960754439,1.51208293277137,0.900011072182198));
#11656=CARTESIAN_POINT('Ctrl Pts',(5.72069615836457,1.85663493780214,0.899990666655967));
#11657=CARTESIAN_POINT('Ctrl Pts',(9.5180705084307,1.59456947801794,0.900005849269565));
#11658=CARTESIAN_POINT('Ctrl Pts',(11.6765943959699,1.38252448313292,0.9));
#11659=CARTESIAN_POINT('Ctrl Pts',(0.287623587302861,1.35283178372728,0.83061654407248));
#11660=CARTESIAN_POINT('Ctrl Pts',(1.89907070881462,1.6612970673762,0.830110312711064));
#11661=CARTESIAN_POINT('Ctrl Pts',(5.72203120258494,2.00791989451774,0.829536565111056));
#11662=CARTESIAN_POINT('Ctrl Pts',(9.52981562096212,1.74434245945332,0.829975639897288));
#11663=CARTESIAN_POINT('Ctrl Pts',(11.6912432102654,1.53175516862908,0.830242007927395));
#11664=CARTESIAN_POINT('Ctrl Pts',(0.276437927844243,1.41141950219787,0.682830994206899));
#11665=CARTESIAN_POINT('Ctrl Pts',(1.89175654834445,1.7202459032803,0.681514651829601));
#11666=CARTESIAN_POINT('Ctrl Pts',(5.72254254462207,2.06699613896002,0.680031275065471));
#11667=CARTESIAN_POINT('Ctrl Pts',(9.53442784766217,1.80334383841306,0.681166806353567));
#11668=CARTESIAN_POINT('Ctrl Pts',(11.6970428895979,1.59083777456472,0.681858145263204));
#11669=CARTESIAN_POINT('Ctrl Pts',(0.275700153393682,1.4152837823473,0.618237860411764));
#11670=CARTESIAN_POINT('Ctrl Pts',(1.89131690864814,1.72383635907408,0.616681840548257));
#11671=CARTESIAN_POINT('Ctrl Pts',(5.72257555688819,2.07025489722917,0.614922376024419));
#11672=CARTESIAN_POINT('Ctrl Pts',(9.53470357301702,1.80685728936816,0.616269329673511));
#11673=CARTESIAN_POINT('Ctrl Pts',(11.6974038588243,1.59451504727786,0.617085749108931));
#11674=CARTESIAN_POINT('Ctrl Pts',(11.6974038588243,1.59451504727786,0.617085749108931));
#11675=CARTESIAN_POINT('Ctrl Pts',(9.53470357301702,1.80685728936816,0.616269329673511));
#11676=CARTESIAN_POINT('Ctrl Pts',(5.72257555688819,2.07025489722917,0.614922376024419));
#11677=CARTESIAN_POINT('Ctrl Pts',(1.89131690864814,1.72383635907408,0.616681840548257));
#11678=CARTESIAN_POINT('Ctrl Pts',(0.275700153393682,1.4152837823473,0.618237860411764));
#11679=CARTESIAN_POINT('Ctrl Pts',(0.3318563713692,1.12115139781563,0.9));
#11680=CARTESIAN_POINT('Ctrl Pts',(1.92849230856897,1.42598364489954,0.9));
#11681=CARTESIAN_POINT('Ctrl Pts',(5.71993880054687,1.76935652211139,0.9));
#11682=CARTESIAN_POINT('Ctrl Pts',(9.51130499016288,1.50815471522196,0.9));
#11683=CARTESIAN_POINT('Ctrl Pts',(11.6681436286308,1.2964346619681,0.9));
#11684=CARTESIAN_POINT('Ctrl Pts',(-0.000343174493958709,1.15350944952984,
-0.00654815942696785));
#11685=CARTESIAN_POINT('Ctrl Pts',(0.0105270529019337,1.14272303380391,
0.200868135340743));
#11686=CARTESIAN_POINT('Ctrl Pts',(0.0213972813757523,1.13193701467556,
0.408284450676511));
#11687=CARTESIAN_POINT('Ctrl Pts',(0.0322675109428289,1.12115139781563,
0.615700786872884));
#11688=CARTESIAN_POINT('Ctrl Pts',(-0.000129060241737355,1.23228777111366,
-0.0024626161135415));
#11689=CARTESIAN_POINT('Ctrl Pts',(0.0107416412387167,1.22148297235423,
0.204952596860618));
#11690=CARTESIAN_POINT('Ctrl Pts',(0.0216107531875107,1.21067920461451,
0.412367946918899));
#11691=CARTESIAN_POINT('Ctrl Pts',(0.0324814606290031,1.19987501734845,
0.61978319007907));
#11692=CARTESIAN_POINT('Ctrl Pts',(0.0574602827844584,1.36931747586956,
0.00164530659801973));
#11693=CARTESIAN_POINT('Ctrl Pts',(0.0683025556324749,1.35848226928888,
0.209060253413207));
#11694=CARTESIAN_POINT('Ctrl Pts',(0.079145272670006,1.34764679267913,0.416475160658282));
#11695=CARTESIAN_POINT('Ctrl Pts',(0.0899872847341513,1.33681188280878,
0.62389013300849));
#11696=CARTESIAN_POINT('Ctrl Pts',(0.185325846363896,1.43651931939441,-0.00156109881554352));
#11697=CARTESIAN_POINT('Ctrl Pts',(0.196119220517603,1.4256988926218,0.205857093047737));
#11698=CARTESIAN_POINT('Ctrl Pts',(0.20691256009293,1.41487906031557,0.413275315721495));
#11699=CARTESIAN_POINT('Ctrl Pts',(0.217705180746507,1.40405902353128,0.620693562444772));
#11700=CARTESIAN_POINT('Ctrl Pts',(0.243371723604776,1.44769625339383,-0.00402191236404));
#11701=CARTESIAN_POINT('Ctrl Pts',(0.254148334883323,1.43689183478419,0.203397976373256));
#11702=CARTESIAN_POINT('Ctrl Pts',(0.264924480472538,1.42608767680315,0.410817900476086));
#11703=CARTESIAN_POINT('Ctrl Pts',(0.275700153393682,1.4152837823473,0.618237860411764));
#11704=CARTESIAN_POINT('Ctrl Pts',(-1.23734572934908E-17,1.15316892111333,
-8.67361737988404E-19));
#11705=CARTESIAN_POINT('Ctrl Pts',(0.0107558359204753,1.14249602316336,
0.205233575389367));
#11706=CARTESIAN_POINT('Ctrl Pts',(0.0215116728964674,1.13182351356624,
0.410467170919192));
#11707=CARTESIAN_POINT('Ctrl Pts',(0.0322675109428289,1.12115139781563,
0.615700786872884));
#11708=CARTESIAN_POINT('Ctrl Pts',(0.275700153393682,1.4152837823473,0.618237860411764));
#11709=CARTESIAN_POINT('Ctrl Pts',(0.264994127943615,1.42601784692504,0.412158538389472));
#11710=CARTESIAN_POINT('Ctrl Pts',(0.254287635915814,1.43675217163244,0.206079251738322));
#11711=CARTESIAN_POINT('Ctrl Pts',(0.243580684154575,1.44748675362873,-1.9298798670242E-17));
#11712=CARTESIAN_POINT('Ctrl Pts',(11.7295909468525,-1.62672708026858,0.));
#11713=CARTESIAN_POINT('Ctrl Pts',(11.7192775324813,-1.61592692249094,0.206079286804135));
#11714=CARTESIAN_POINT('Ctrl Pts',(11.70896411811,-1.6051267647133,0.41215857360827));
#11715=CARTESIAN_POINT('Ctrl Pts',(11.6986507037388,-1.59432660693566,0.618237860412405));
#11716=CARTESIAN_POINT('Ctrl Pts',(7.90092085928651,-2.00057770191527,0.));
#11717=CARTESIAN_POINT('Ctrl Pts',(7.89749915175266,-1.98977754413763,0.206079286804135));
#11718=CARTESIAN_POINT('Ctrl Pts',(7.89407744421881,-1.97897738636,0.41215857360827));
#11719=CARTESIAN_POINT('Ctrl Pts',(7.89065573668496,-1.96817722858236,0.618237860412405));
#11720=CARTESIAN_POINT('Ctrl Pts',(4.07225077172054,-2.17467835246083,0.));
#11721=CARTESIAN_POINT('Ctrl Pts',(4.07572077102407,-2.16387819468319,0.206079286804135));
#11722=CARTESIAN_POINT('Ctrl Pts',(4.07919077032759,-2.15307803690555,0.41215857360827));
#11723=CARTESIAN_POINT('Ctrl Pts',(4.08266076963111,-2.14227787912792,0.618237860412405));
#11724=CARTESIAN_POINT('Ctrl Pts',(0.243580684154574,-1.44748675362873,
0.));
#11725=CARTESIAN_POINT('Ctrl Pts',(0.253942390295469,-1.43668659585109,
0.206079286804135));
#11726=CARTESIAN_POINT('Ctrl Pts',(0.264304096436365,-1.42588643807345,
0.41215857360827));
#11727=CARTESIAN_POINT('Ctrl Pts',(0.27466580257726,-1.41508628029581,0.618237860412405));
#11728=CARTESIAN_POINT('Origin',(0.,-1.4,0.));
#11729=CARTESIAN_POINT('Origin',(6.08012166120517,1.06803409199199E-16,
0.9));
#11730=CARTESIAN_POINT('Ctrl Pts',(0.243580684154574,1.44748675362873,0.));
#11731=CARTESIAN_POINT('Ctrl Pts',(0.253942390295469,1.43668659585109,0.206079286804135));
#11732=CARTESIAN_POINT('Ctrl Pts',(0.264304096436365,1.42588643807345,0.41215857360827));
#11733=CARTESIAN_POINT('Ctrl Pts',(0.27466580257726,1.41508628029581,0.618237860412405));
#11734=CARTESIAN_POINT('Ctrl Pts',(4.07225077172054,2.17467835246083,0.));
#11735=CARTESIAN_POINT('Ctrl Pts',(4.07572077102407,2.16387819468319,0.206079286804135));
#11736=CARTESIAN_POINT('Ctrl Pts',(4.07919077032759,2.15307803690555,0.41215857360827));
#11737=CARTESIAN_POINT('Ctrl Pts',(4.08266076963111,2.14227787912792,0.618237860412405));
#11738=CARTESIAN_POINT('Ctrl Pts',(7.90092085928651,2.00057770191527,0.));
#11739=CARTESIAN_POINT('Ctrl Pts',(7.89749915175266,1.98977754413763,0.206079286804135));
#11740=CARTESIAN_POINT('Ctrl Pts',(7.89407744421881,1.97897738636,0.41215857360827));
#11741=CARTESIAN_POINT('Ctrl Pts',(7.89065573668496,1.96817722858236,0.618237860412405));
#11742=CARTESIAN_POINT('Ctrl Pts',(11.7295909468525,1.62672708026858,0.));
#11743=CARTESIAN_POINT('Ctrl Pts',(11.7192775324813,1.61592692249094,0.206079286804135));
#11744=CARTESIAN_POINT('Ctrl Pts',(11.70896411811,1.6051267647133,0.41215857360827));
#11745=CARTESIAN_POINT('Ctrl Pts',(11.6986507037388,1.59432660693566,0.618237860412405));
#11746=CARTESIAN_POINT('Origin',(12.,1.6,0.));
#11747=CARTESIAN_POINT('',(0.,0.,0.));
#11748=CARTESIAN_POINT('Origin',(9.,-1.,0.8));
#11749=CARTESIAN_POINT('',(8.85,-1.,0.9));
#11750=CARTESIAN_POINT('Origin',(9.,-1.,0.9));
#11751=CARTESIAN_POINT('',(8.85,-1.,0.7));
#11752=CARTESIAN_POINT('',(8.85,-1.,0.8));
#11753=CARTESIAN_POINT('Origin',(9.,-1.,0.7));
#11754=CARTESIAN_POINT('Origin',(3.,-1.,0.8));
#11755=CARTESIAN_POINT('',(2.85,-1.,0.9));
#11756=CARTESIAN_POINT('Origin',(3.,-1.,0.9));
#11757=CARTESIAN_POINT('',(2.85,-1.,0.7));
#11758=CARTESIAN_POINT('',(2.85,-1.,0.8));
#11759=CARTESIAN_POINT('Origin',(3.,-1.,0.7));
#11760=CARTESIAN_POINT('Origin',(3.,1.,0.8));
#11761=CARTESIAN_POINT('',(2.85,1.,0.9));
#11762=CARTESIAN_POINT('Origin',(3.,1.,0.9));
#11763=CARTESIAN_POINT('',(2.85,1.,0.7));
#11764=CARTESIAN_POINT('',(2.85,1.,0.8));
#11765=CARTESIAN_POINT('Origin',(3.,1.,0.7));
#11766=CARTESIAN_POINT('Origin',(9.,1.,0.8));
#11767=CARTESIAN_POINT('',(8.85,1.,0.9));
#11768=CARTESIAN_POINT('Origin',(9.,1.,0.9));
#11769=CARTESIAN_POINT('',(8.85,1.,0.7));
#11770=CARTESIAN_POINT('',(8.85,1.,0.8));
#11771=CARTESIAN_POINT('Origin',(9.,1.,0.7));
#11772=CARTESIAN_POINT('Origin',(10.1732050807569,0.3,0.9));
#11773=CARTESIAN_POINT('',(10.1732050807569,0.3,0.9));
#11774=CARTESIAN_POINT('',(10.3464101615138,0.,0.9));
#11775=CARTESIAN_POINT('',(9.72652155859676,1.07367855528516,0.9));
#11776=CARTESIAN_POINT('',(10.1732050807569,0.3,0.6));
#11777=CARTESIAN_POINT('',(10.1732050807569,0.3,0.9));
#11778=CARTESIAN_POINT('',(10.3464101615138,0.,0.6));
#11779=CARTESIAN_POINT('',(10.3464101615138,0.,0.6));
#11780=CARTESIAN_POINT('',(10.3464101615138,0.,0.9));
#11781=CARTESIAN_POINT('Origin',(9.82679491924311,0.3,0.9));
#11782=CARTESIAN_POINT('',(9.82679491924311,0.3,0.9));
#11783=CARTESIAN_POINT('',(7.95345829022414,0.3,0.9));
#11784=CARTESIAN_POINT('',(9.82679491924311,0.3,0.6));
#11785=CARTESIAN_POINT('',(9.82679491924311,0.3,0.9));
#11786=CARTESIAN_POINT('',(10.1732050807569,0.3,0.6));
#11787=CARTESIAN_POINT('Origin',(9.65358983848622,5.55111512312578E-17,
0.9));
#11788=CARTESIAN_POINT('',(9.65358983848622,4.24230095489963E-17,0.9));
#11789=CARTESIAN_POINT('',(9.2069063163261,-0.773678555285165,0.9));
#11790=CARTESIAN_POINT('',(9.65358983848622,5.55111512312578E-17,0.6));
#11791=CARTESIAN_POINT('',(9.65358983848622,4.24230095489963E-17,0.9));
#11792=CARTESIAN_POINT('',(9.82679491924311,0.3,0.6));
#11793=CARTESIAN_POINT('Origin',(9.82679491924311,-0.3,0.9));
#11794=CARTESIAN_POINT('',(9.82679491924311,-0.3,0.9));
#11795=CARTESIAN_POINT('',(9.29350885670454,0.623678555285165,0.9));
#11796=CARTESIAN_POINT('',(9.82679491924311,-0.3,0.6));
#11797=CARTESIAN_POINT('',(9.82679491924311,-0.3,0.9));
#11798=CARTESIAN_POINT('',(9.65358983848622,4.24230095489963E-17,0.6));
#11799=CARTESIAN_POINT('Origin',(10.1732050807569,-0.3,0.9));
#11800=CARTESIAN_POINT('',(10.1732050807569,-0.3,0.9));
#11801=CARTESIAN_POINT('',(8.12666337098103,-0.3,0.9));
#11802=CARTESIAN_POINT('',(10.1732050807569,-0.3,0.6));
#11803=CARTESIAN_POINT('',(10.1732050807569,-0.3,0.9));
#11804=CARTESIAN_POINT('',(9.82679491924311,-0.3,0.6));
#11805=CARTESIAN_POINT('Origin',(10.3464101615138,0.,0.9));
#11806=CARTESIAN_POINT('',(9.8131240989752,-0.923678555285165,0.9));
#11807=CARTESIAN_POINT('',(10.1732050807569,-0.3,0.6));
#11808=CARTESIAN_POINT('Origin',(10.,5.55111512312578E-17,0.6));
#11809=CARTESIAN_POINT('',(9.83,-2.0818995585505E-17,0.6));
#11810=CARTESIAN_POINT('Origin',(10.,0.,0.6));
#11811=CARTESIAN_POINT('Origin',(2.17320508075689,0.3,0.9));
#11812=CARTESIAN_POINT('',(2.17320508075689,0.3,0.9));
#11813=CARTESIAN_POINT('',(2.34641016151378,0.,0.9));
#11814=CARTESIAN_POINT('',(2.72652155859676,-0.65837225228371,0.9));
#11815=CARTESIAN_POINT('',(2.17320508075689,0.3,0.6));
#11816=CARTESIAN_POINT('',(2.17320508075689,0.3,0.9));
#11817=CARTESIAN_POINT('',(2.34641016151378,0.,0.6));
#11818=CARTESIAN_POINT('',(2.34641016151378,0.,0.6));
#11819=CARTESIAN_POINT('',(2.34641016151378,0.,0.9));
#11820=CARTESIAN_POINT('Origin',(1.82679491924311,0.3,0.9));
#11821=CARTESIAN_POINT('',(1.82679491924311,0.3,0.9));
#11822=CARTESIAN_POINT('',(3.95345829022414,0.3,0.9));
#11823=CARTESIAN_POINT('',(1.82679491924311,0.3,0.6));
#11824=CARTESIAN_POINT('',(1.82679491924311,0.3,0.9));
#11825=CARTESIAN_POINT('',(2.17320508075689,0.3,0.6));
#11826=CARTESIAN_POINT('Origin',(1.65358983848622,5.55111512312578E-17,
0.9));
#11827=CARTESIAN_POINT('',(1.65358983848622,4.24230095489963E-17,0.9));
#11828=CARTESIAN_POINT('',(2.20690631632609,0.958372252283711,0.9));
#11829=CARTESIAN_POINT('',(1.65358983848622,5.55111512312578E-17,0.6));
#11830=CARTESIAN_POINT('',(1.65358983848622,4.24230095489963E-17,0.9));
#11831=CARTESIAN_POINT('',(1.82679491924311,0.3,0.6));
#11832=CARTESIAN_POINT('Origin',(1.82679491924311,-0.3,0.9));
#11833=CARTESIAN_POINT('',(1.82679491924311,-0.3,0.9));
#11834=CARTESIAN_POINT('',(2.29350885670453,-1.10837225228371,0.9));
#11835=CARTESIAN_POINT('',(1.82679491924311,-0.3,0.6));
#11836=CARTESIAN_POINT('',(1.82679491924311,-0.3,0.9));
#11837=CARTESIAN_POINT('',(1.65358983848622,4.24230095489963E-17,0.6));
#11838=CARTESIAN_POINT('Origin',(2.17320508075689,-0.3,0.9));
#11839=CARTESIAN_POINT('',(2.17320508075689,-0.3,0.9));
#11840=CARTESIAN_POINT('',(4.12666337098103,-0.3,0.9));
#11841=CARTESIAN_POINT('',(2.17320508075689,-0.3,0.6));
#11842=CARTESIAN_POINT('',(2.17320508075689,-0.3,0.9));
#11843=CARTESIAN_POINT('',(1.82679491924311,-0.3,0.6));
#11844=CARTESIAN_POINT('Origin',(2.34641016151378,0.,0.9));
#11845=CARTESIAN_POINT('',(2.8131240989752,0.80837225228371,0.9));
#11846=CARTESIAN_POINT('',(2.17320508075689,-0.3,0.6));
#11847=CARTESIAN_POINT('Origin',(2.,5.55111512312578E-17,0.6));
#11848=CARTESIAN_POINT('',(1.83,-2.0818995585505E-17,0.6));
#11849=CARTESIAN_POINT('Origin',(2.,0.,0.6));
#11850=CARTESIAN_POINT('Origin',(2.,0.,0.45));
#11851=CARTESIAN_POINT('',(1.83,-2.0818995585505E-17,0.32));
#11852=CARTESIAN_POINT('',(1.83,2.0818995585505E-17,0.45));
#11853=CARTESIAN_POINT('Origin',(2.,0.,0.32));
#11854=CARTESIAN_POINT('Origin',(10.,0.,0.45));
#11855=CARTESIAN_POINT('',(9.83,-2.0818995585505E-17,0.32));
#11856=CARTESIAN_POINT('',(9.83,2.0818995585505E-17,0.45));
#11857=CARTESIAN_POINT('Origin',(10.,0.,0.32));
#11858=CARTESIAN_POINT('Origin',(11.2,-0.62,0.32));
#11859=CARTESIAN_POINT('',(0.200274469199584,-0.62,0.));
#11860=CARTESIAN_POINT('',(0.217044958570157,-0.62,0.32));
#11861=CARTESIAN_POINT('',(0.223426876981161,-0.62,0.441774257530303));
#11862=CARTESIAN_POINT('',(0.,-0.62,0.));
#11863=CARTESIAN_POINT('',(8.63987299740311,-0.62,0.));
#11864=CARTESIAN_POINT('',(0.0167704893705732,-0.62,0.32));
#11865=CARTESIAN_POINT('',(0.0237009700302462,-0.62,0.452241448778892));
#11866=CARTESIAN_POINT('',(-0.1,-0.62,0.32));
#11867=CARTESIAN_POINT('Origin',(11.2,-0.62,0.32));
#11868=CARTESIAN_POINT('',(0.9,-0.62,0.32));
#11869=CARTESIAN_POINT('',(0.9,-0.62,0.));
#11870=CARTESIAN_POINT('',(0.9,-0.62,0.16));
#11871=CARTESIAN_POINT('',(1.1,-0.62,0.32));
#11872=CARTESIAN_POINT('',(-0.1,-0.62,0.32));
#11873=CARTESIAN_POINT('',(1.1,-0.62,0.));
#11874=CARTESIAN_POINT('',(1.1,-0.62,0.16));
#11875=CARTESIAN_POINT('',(8.63987299740311,-0.62,0.));
#11876=CARTESIAN_POINT('Origin',(11.2,-0.62,0.32));
#11877=CARTESIAN_POINT('',(3.9,-0.62,0.32));
#11878=CARTESIAN_POINT('',(3.9,-0.62,0.));
#11879=CARTESIAN_POINT('',(3.9,-0.62,0.16));
#11880=CARTESIAN_POINT('',(4.1,-0.62,0.32));
#11881=CARTESIAN_POINT('',(-0.1,-0.62,0.32));
#11882=CARTESIAN_POINT('',(4.1,-0.62,0.));
#11883=CARTESIAN_POINT('',(4.1,-0.62,0.16));
#11884=CARTESIAN_POINT('',(8.63987299740311,-0.62,0.));
#11885=CARTESIAN_POINT('Origin',(11.2,-0.62,0.32));
#11886=CARTESIAN_POINT('',(7.9,-0.62,0.32));
#11887=CARTESIAN_POINT('',(7.9,-0.62,0.));
#11888=CARTESIAN_POINT('',(7.9,-0.62,0.16));
#11889=CARTESIAN_POINT('',(8.1,-0.62,0.32));
#11890=CARTESIAN_POINT('',(-0.1,-0.62,0.32));
#11891=CARTESIAN_POINT('',(8.1,-0.62,0.));
#11892=CARTESIAN_POINT('',(8.1,-0.62,0.16));
#11893=CARTESIAN_POINT('',(8.63987299740311,-0.62,0.));
#11894=CARTESIAN_POINT('Origin',(-0.0999999999999996,0.62,0.32));
#11895=CARTESIAN_POINT('',(0.217044958570158,0.62,0.32));
#11896=CARTESIAN_POINT('',(0.200274469199586,0.62,0.));
#11897=CARTESIAN_POINT('',(0.207951231396534,0.62,0.146481348799182));
#11898=CARTESIAN_POINT('',(0.0167704893705736,0.62,0.32));
#11899=CARTESIAN_POINT('',(11.2,0.62,0.32));
#11900=CARTESIAN_POINT('',(0.,0.62,0.));
#11901=CARTESIAN_POINT('',(0.00822532444561912,0.62,0.156948540047771));
#11902=CARTESIAN_POINT('',(2.98987299740311,0.62,0.));
#11903=CARTESIAN_POINT('Origin',(-0.0999999999999996,0.62,0.32));
#11904=CARTESIAN_POINT('',(0.9,0.62,0.));
#11905=CARTESIAN_POINT('',(0.9,0.62,0.32));
#11906=CARTESIAN_POINT('',(0.9,0.62,0.16));
#11907=CARTESIAN_POINT('',(1.1,0.62,0.));
#11908=CARTESIAN_POINT('',(2.98987299740311,0.62,0.));
#11909=CARTESIAN_POINT('',(1.1,0.62,0.32));
#11910=CARTESIAN_POINT('',(1.1,0.62,0.16));
#11911=CARTESIAN_POINT('',(11.2,0.62,0.32));
#11912=CARTESIAN_POINT('Origin',(-0.0999999999999996,0.62,0.32));
#11913=CARTESIAN_POINT('',(3.9,0.62,0.));
#11914=CARTESIAN_POINT('',(3.9,0.62,0.32));
#11915=CARTESIAN_POINT('',(3.9,0.62,0.16));
#11916=CARTESIAN_POINT('',(4.1,0.62,0.));
#11917=CARTESIAN_POINT('',(2.98987299740311,0.62,0.));
#11918=CARTESIAN_POINT('',(4.1,0.62,0.32));
#11919=CARTESIAN_POINT('',(4.1,0.62,0.16));
#11920=CARTESIAN_POINT('',(11.2,0.62,0.32));
#11921=CARTESIAN_POINT('Origin',(5.55,0.,0.32));
#11922=CARTESIAN_POINT('',(1.6,-4.89858719658941E-17,0.32));
#11923=CARTESIAN_POINT('Origin',(2.,0.,0.32));
#11924=CARTESIAN_POINT('Origin',(5.55,0.,0.32));
#11925=CARTESIAN_POINT('',(9.6,-4.89858719658942E-17,0.32));
#11926=CARTESIAN_POINT('Origin',(10.,0.,0.32));
#11927=CARTESIAN_POINT('Origin',(5.55,0.,0.32));
#11928=CARTESIAN_POINT('',(0.217044958570157,-0.7,0.32));
#11929=CARTESIAN_POINT('',(0.0167704893705731,-0.7,0.32));
#11930=CARTESIAN_POINT('Origin',(5.55,0.,0.32));
#11931=CARTESIAN_POINT('',(0.9,0.724814814814815,0.32));
#11932=CARTESIAN_POINT('',(1.1,-0.724814814814815,0.32));
#11933=CARTESIAN_POINT('Origin',(5.55,0.,0.32));
#11934=CARTESIAN_POINT('',(3.9,0.883148148148148,0.32));
#11935=CARTESIAN_POINT('',(4.1,-0.883148148148148,0.32));
#11936=CARTESIAN_POINT('Origin',(5.55,0.,0.32));
#11937=CARTESIAN_POINT('',(7.9,0.62,0.32));
#11938=CARTESIAN_POINT('',(7.9,0.886851851851852,0.32));
#11939=CARTESIAN_POINT('',(8.1,0.62,0.32));
#11940=CARTESIAN_POINT('',(11.2,0.62,0.32));
#11941=CARTESIAN_POINT('',(8.1,-0.886851851851852,0.32));
#11942=CARTESIAN_POINT('Origin',(-0.0999999999999996,0.62,0.32));
#11943=CARTESIAN_POINT('',(7.9,0.62,0.));
#11944=CARTESIAN_POINT('',(7.9,0.62,0.16));
#11945=CARTESIAN_POINT('',(8.1,0.62,0.));
#11946=CARTESIAN_POINT('',(2.98987299740311,0.62,0.));
#11947=CARTESIAN_POINT('',(8.1,0.62,0.16));
#11948=CARTESIAN_POINT('Origin',(11.2,1.53779953703704,0.));
#11949=CARTESIAN_POINT('',(11.2,1.47592264243751,0.));
#11950=CARTESIAN_POINT('',(11.2,-1.47592264243751,0.));
#11951=CARTESIAN_POINT('',(11.2,1.53779953703704,0.));
#11952=CARTESIAN_POINT('',(11.2,-1.44160695250311,0.605635447211793));
#11953=CARTESIAN_POINT('Ctrl Pts',(11.2,-1.44160695250311,0.605635447211793));
#11954=CARTESIAN_POINT('Ctrl Pts',(11.2,-1.44733381480461,0.504614841520655));
#11955=CARTESIAN_POINT('Ctrl Pts',(11.2,-1.45305922122436,0.403593539811385));
#11956=CARTESIAN_POINT('Ctrl Pts',(11.2,-1.46449774781658,0.201715464978033));
#11957=CARTESIAN_POINT('Ctrl Pts',(11.2,-1.47021094199039,0.100857470386242));
#11958=CARTESIAN_POINT('Ctrl Pts',(11.2,-1.47592264243751,0.));
#11959=CARTESIAN_POINT('',(11.2,-1.3413305091784,0.7));
#11960=CARTESIAN_POINT('Ctrl Pts',(11.2,-1.34133050917871,0.7));
#11961=CARTESIAN_POINT('Ctrl Pts',(11.2,-1.34927184579059,0.7));
#11962=CARTESIAN_POINT('Ctrl Pts',(11.1999981201149,-1.35715077597425,0.699006225306896));
#11963=CARTESIAN_POINT('Ctrl Pts',(11.1999964866412,-1.36482619101963,0.697118463987577));
#11964=CARTESIAN_POINT('Ctrl Pts',(11.1999955714568,-1.36912648693643,0.696060810134936));
#11965=CARTESIAN_POINT('Ctrl Pts',(11.1999947385598,-1.37336294684024,0.694721504600825));
#11966=CARTESIAN_POINT('Ctrl Pts',(11.1999942054834,-1.37750904339755,0.693111246644731));
#11967=CARTESIAN_POINT('Ctrl Pts',(11.1999932489192,-1.38494889279378,0.690221763364053));
#11968=CARTESIAN_POINT('Ctrl Pts',(11.1999934335488,-1.39201911070639,0.686493604183975));
#11969=CARTESIAN_POINT('Ctrl Pts',(11.1999946360439,-1.39857284316731,0.682006025455124));
#11970=CARTESIAN_POINT('Ctrl Pts',(11.1999952980149,-1.40218065925828,0.679535622697003));
#11971=CARTESIAN_POINT('Ctrl Pts',(11.1999962427007,-1.40563167682227,0.676834205328214));
#11972=CARTESIAN_POINT('Ctrl Pts',(11.1999970766466,-1.40889738828709,0.673909521834337));
#11973=CARTESIAN_POINT('Ctrl Pts',(11.1999978839828,-1.41205889660265,0.671078159882768));
#11974=CARTESIAN_POINT('Ctrl Pts',(11.1999985961359,-1.41502771690814,0.668054510912379));
#11975=CARTESIAN_POINT('Ctrl Pts',(11.1999985943254,-1.41778154893794,0.664849526385156));
#11976=CARTESIAN_POINT('Ctrl Pts',(11.1999985909468,-1.42292039881534,0.658868793295219));
#11977=CARTESIAN_POINT('Ctrl Pts',(11.1999963776609,-1.42731355725865,0.652257958652517));
#11978=CARTESIAN_POINT('Ctrl Pts',(11.1999956369,-1.43089859237711,0.645180832176479));
#11979=CARTESIAN_POINT('Ctrl Pts',(11.1999955610412,-1.43126572346771,0.644456088045497));
#11980=CARTESIAN_POINT('Ctrl Pts',(11.1999954968237,-1.43162433912915,0.643726434786758));
#11981=CARTESIAN_POINT('Ctrl Pts',(11.1999954455063,-1.43197434355081,0.642992037678167));
#11982=CARTESIAN_POINT('Ctrl Pts',(11.1999949451572,-1.43538691836834,0.635831599341589));
#11983=CARTESIAN_POINT('Ctrl Pts',(11.1999960935741,-1.43794480573841,0.628305806294037));
#11984=CARTESIAN_POINT('Ctrl Pts',(11.1999977538348,-1.43959303921538,0.620581877990282));
#11985=CARTESIAN_POINT('Ctrl Pts',(11.1999988103007,-1.44064185190664,0.615666946856702));
#11986=CARTESIAN_POINT('Ctrl Pts',(11.1999999935832,-1.44132148083109,0.610671141596651));
#11987=CARTESIAN_POINT('Ctrl Pts',(11.1999999950647,-1.44160695392865,0.605635447210179));
#11988=CARTESIAN_POINT('',(11.2,1.34133050917871,0.7));
#11989=CARTESIAN_POINT('',(11.2,0.768899768518519,0.7));
#11990=CARTESIAN_POINT('',(11.2,1.44160695250311,0.605635447211793));
#11991=CARTESIAN_POINT('Ctrl Pts',(11.1999999950647,1.44160695392865,0.605635447210179));
#11992=CARTESIAN_POINT('Ctrl Pts',(11.1999999927383,1.44115867123275,0.613543073794128));
#11993=CARTESIAN_POINT('Ctrl Pts',(11.199997327584,1.43974095598264,0.62135504174347));
#11994=CARTESIAN_POINT('Ctrl Pts',(11.1999961426836,1.43743894790867,0.628911795513178));
#11995=CARTESIAN_POINT('Ctrl Pts',(11.1999954950047,1.43618064644969,0.633042395401645));
#11996=CARTESIAN_POINT('Ctrl Pts',(11.1999951984378,1.4346571631488,0.63709676955888));
#11997=CARTESIAN_POINT('Ctrl Pts',(11.1999953420225,1.43287614971348,0.641047046155727));
#11998=CARTESIAN_POINT('Ctrl Pts',(11.1999956050472,1.42961361303411,0.648283331988978));
#11999=CARTESIAN_POINT('Ctrl Pts',(11.1999975633633,1.42552584716917,0.655091209244077));
#12000=CARTESIAN_POINT('Ctrl Pts',(11.1999983488166,1.42067941835906,0.661308913390503));
#12001=CARTESIAN_POINT('Ctrl Pts',(11.1999985007599,1.41974189284539,0.662511707551344));
#12002=CARTESIAN_POINT('Ctrl Pts',(11.1999985958742,1.41877583892185,0.663692344451305));
#12003=CARTESIAN_POINT('Ctrl Pts',(11.1999985956185,1.41778154881703,0.664849526385225));
#12004=CARTESIAN_POINT('Ctrl Pts',(11.199998595152,1.41596832836708,0.666959801783445));
#12005=CARTESIAN_POINT('Ctrl Pts',(11.1999982799021,1.41406123008998,0.668992111776222));
#12006=CARTESIAN_POINT('Ctrl Pts',(11.1999978412043,1.41206657472189,0.670943322037058));
#12007=CARTESIAN_POINT('Ctrl Pts',(11.1999965906985,1.40638082038708,0.676505236328724));
#12008=CARTESIAN_POINT('Ctrl Pts',(11.1999945592311,1.40005057587654,0.681348449922958));
#12009=CARTESIAN_POINT('Ctrl Pts',(11.1999938793032,1.39324090595796,0.685420973467861));
#12010=CARTESIAN_POINT('Ctrl Pts',(11.1999934424014,1.38886521116801,0.68803785802621));
#12011=CARTESIAN_POINT('Ctrl Pts',(11.1999934711477,1.38429057260668,0.690335857752236));
#12012=CARTESIAN_POINT('Ctrl Pts',(11.1999939665515,1.37955471147715,0.692291686537622));
#12013=CARTESIAN_POINT('Ctrl Pts',(11.1999947349645,1.37220899016913,0.695325342464331));
#12014=CARTESIAN_POINT('Ctrl Pts',(11.1999966395725,1.36455954597093,0.697503651902993));
#12015=CARTESIAN_POINT('Ctrl Pts',(11.1999981885915,1.35675452105021,0.698758058199902));
#12016=CARTESIAN_POINT('Ctrl Pts',(11.1999991983045,1.35166689148409,0.699575730741489));
#12017=CARTESIAN_POINT('Ctrl Pts',(11.2,1.34651254223162,0.7));
#12018=CARTESIAN_POINT('Ctrl Pts',(11.2,1.34133050917871,0.7));
#12019=CARTESIAN_POINT('Ctrl Pts',(11.2,1.47592264243751,0.));
#12020=CARTESIAN_POINT('Ctrl Pts',(11.2,1.47021025951677,0.100869521536925));
#12021=CARTESIAN_POINT('Ctrl Pts',(11.2,1.4644963825062,0.20173956751342));
#12022=CARTESIAN_POINT('Ctrl Pts',(11.2,1.45305785520703,0.403617642353031));
#12023=CARTESIAN_POINT('Ctrl Pts',(11.2,1.44733313162379,0.50462689268162));
#12024=CARTESIAN_POINT('Ctrl Pts',(11.2,1.44160695250311,0.605635447211793));
#12025=CARTESIAN_POINT('Origin',(8.1,-1.7737037037037,0.));
#12026=CARTESIAN_POINT('',(8.1,1.69866351109718,0.));
#12027=CARTESIAN_POINT('',(8.1,-1.7737037037037,0.));
#12028=CARTESIAN_POINT('',(8.1,1.66641703131627,0.605314487869832));
#12029=CARTESIAN_POINT('Ctrl Pts',(8.1,1.66641703131627,0.605314487869832));
#12030=CARTESIAN_POINT('Ctrl Pts',(8.1,1.67178339996556,0.504592280948055));
#12031=CARTESIAN_POINT('Ctrl Pts',(8.1,1.67714947719849,0.403869246528492));
#12032=CARTESIAN_POINT('Ctrl Pts',(8.1,1.68789827452893,0.202098297941347));
#12033=CARTESIAN_POINT('Ctrl Pts',(8.1,1.69328107955938,0.101048748975501));
#12034=CARTESIAN_POINT('Ctrl Pts',(8.1,1.69866351109718,0.));
#12035=CARTESIAN_POINT('',(8.1,1.56644778183753,0.7));
#12036=CARTESIAN_POINT('Ctrl Pts',(8.0999999986552,1.56644778212326,0.7));
#12037=CARTESIAN_POINT('Ctrl Pts',(8.10000000155239,1.57436337254628,0.699999999341293));
#12038=CARTESIAN_POINT('Ctrl Pts',(8.09999905041684,1.58221543358893,0.699005989267703));
#12039=CARTESIAN_POINT('Ctrl Pts',(8.09999821745812,1.58986365929578,0.697118696434997));
#12040=CARTESIAN_POINT('Ctrl Pts',(8.099997748439,1.59417019217574,0.69605600700222));
#12041=CARTESIAN_POINT('Ctrl Pts',(8.09999731997616,1.59841215407948,0.694709061504878));
#12042=CARTESIAN_POINT('Ctrl Pts',(8.09999704681388,1.60256279759721,0.693088866918468));
#12043=CARTESIAN_POINT('Ctrl Pts',(8.09999655811104,1.60998853482381,0.690190246691698));
#12044=CARTESIAN_POINT('Ctrl Pts',(8.09999665589197,1.61704187682962,0.686451534538094));
#12045=CARTESIAN_POINT('Ctrl Pts',(8.09999726576867,1.62357667434142,0.681954089017224));
#12046=CARTESIAN_POINT('Ctrl Pts',(8.09999760196939,1.62717904774802,0.679474826559159));
#12047=CARTESIAN_POINT('Ctrl Pts',(8.09999808150314,1.6306235748906,0.676764109620253));
#12048=CARTESIAN_POINT('Ctrl Pts',(8.09999850764167,1.63388182210815,0.673830012183301));
#12049=CARTESIAN_POINT('Ctrl Pts',(8.09999892160867,1.637047006066,0.670979719520364));
#12050=CARTESIAN_POINT('Ctrl Pts',(8.09999928906958,1.640017230617,0.667935813742119));
#12051=CARTESIAN_POINT('Ctrl Pts',(8.09999928944056,1.64277007752663,0.664709670235875));
#12052=CARTESIAN_POINT('Ctrl Pts',(8.09999929012967,1.64788359851353,0.658716982277737));
#12053=CARTESIAN_POINT('Ctrl Pts',(8.09999816327153,1.65225000627493,0.652096887528603));
#12054=CARTESIAN_POINT('Ctrl Pts',(8.09999778355904,1.65580927004486,0.645014643130784));
#12055=CARTESIAN_POINT('Ctrl Pts',(8.09999774450894,1.65617530914943,0.644286296325024));
#12056=CARTESIAN_POINT('Ctrl Pts',(8.09999771143612,1.65653277094855,0.643553041785202));
#12057=CARTESIAN_POINT('Ctrl Pts',(8.0999976850083,1.65688156115921,0.642815048027137));
#12058=CARTESIAN_POINT('Ctrl Pts',(8.09999742811004,1.66027206465027,0.635641192980042));
#12059=CARTESIAN_POINT('Ctrl Pts',(8.09999800724182,1.66280786743682,0.628104262855387));
#12060=CARTESIAN_POINT('Ctrl Pts',(8.09999885110511,1.66443535430957,0.620372450280339));
#12061=CARTESIAN_POINT('Ctrl Pts',(8.09999939164969,1.6654778563549,0.615419764910946));
#12062=CARTESIAN_POINT('Ctrl Pts',(8.1,1.66614680274328,0.610386449940169));
#12063=CARTESIAN_POINT('Ctrl Pts',(8.1,1.66641703131627,0.605314487869832));
#12064=CARTESIAN_POINT('',(8.1,-1.56644778183827,0.7));
#12065=CARTESIAN_POINT('',(8.1,-0.886851851851852,0.7));
#12066=CARTESIAN_POINT('',(8.1,-1.66641703131627,0.605314487869832));
#12067=CARTESIAN_POINT('Ctrl Pts',(8.1,-1.66641703131627,0.605314487869832));
#12068=CARTESIAN_POINT('Ctrl Pts',(8.1,-1.66599546653325,0.613226902778437));
#12069=CARTESIAN_POINT('Ctrl Pts',(8.09999864563672,-1.66460605882141,0.621047760783158));
#12070=CARTESIAN_POINT('Ctrl Pts',(8.09999804140045,-1.66233302739118,0.628616817026045));
#12071=CARTESIAN_POINT('Ctrl Pts',(8.09999770486592,-1.66106704316887,0.632832467392296));
#12072=CARTESIAN_POINT('Ctrl Pts',(8.0999975536836,-1.65952595995304,0.636970042829054));
#12073=CARTESIAN_POINT('Ctrl Pts',(8.09999763427866,-1.65771765414013,0.640999885518982));
#12074=CARTESIAN_POINT('Ctrl Pts',(8.09999777898787,-1.65447082344915,0.64823550729937));
#12075=CARTESIAN_POINT('Ctrl Pts',(8.09999878245444,-1.65040085231772,0.655045563401426));
#12076=CARTESIAN_POINT('Ctrl Pts',(8.09999917121848,-1.64557198994432,0.661267087195486));
#12077=CARTESIAN_POINT('Ctrl Pts',(8.09999924425118,-1.6446648462537,0.662435854416292));
#12078=CARTESIAN_POINT('Ctrl Pts',(8.09999928944999,-1.64373079085321,0.663583781603691));
#12079=CARTESIAN_POINT('Ctrl Pts',(8.09999928890117,-1.64277007755202,0.664709670235858));
#12080=CARTESIAN_POINT('Ctrl Pts',(8.09999928782175,-1.64088054556816,0.666924069243459));
#12081=CARTESIAN_POINT('Ctrl Pts',(8.09999911129818,-1.63888792496677,0.66905326411728));
#12082=CARTESIAN_POINT('Ctrl Pts',(8.09999887085824,-1.63679941630975,0.671093569621172));
#12083=CARTESIAN_POINT('Ctrl Pts',(8.09999821641022,-1.6311147520694,0.676647030794692));
#12084=CARTESIAN_POINT('Ctrl Pts',(8.0999972000003,-1.62478663867955,0.681482189379454));
#12085=CARTESIAN_POINT('Ctrl Pts',(8.09999686812141,-1.6179789612855,0.685544965666037));
#12086=CARTESIAN_POINT('Ctrl Pts',(8.09999665686968,-1.61364565292072,0.68813105508359));
#12087=CARTESIAN_POINT('Ctrl Pts',(8.09999667786582,-1.6091170759025,0.690403516124292));
#12088=CARTESIAN_POINT('Ctrl Pts',(8.0999969341683,-1.60442977212996,0.692339085768374));
#12089=CARTESIAN_POINT('Ctrl Pts',(8.09999733452329,-1.59710801128849,0.695362524980696));
#12090=CARTESIAN_POINT('Ctrl Pts',(8.09999831212369,-1.58948382509795,0.697531565976904));
#12091=CARTESIAN_POINT('Ctrl Pts',(8.09999909563861,-1.58170429192971,0.698776637084609));
#12092=CARTESIAN_POINT('Ctrl Pts',(8.09999960249138,-1.57667174192468,0.69958206878261));
#12093=CARTESIAN_POINT('Ctrl Pts',(8.1000000005313,-1.5715735875011,0.699999999573449));
#12094=CARTESIAN_POINT('Ctrl Pts',(8.0999999986552,-1.56644778212326,0.7));
#12095=CARTESIAN_POINT('',(8.1,-1.69866351109718,0.));
#12096=CARTESIAN_POINT('Ctrl Pts',(8.1,-1.69866351109718,0.));
#12097=CARTESIAN_POINT('Ctrl Pts',(8.1,-1.69328105674055,0.101049177371948));
#12098=CARTESIAN_POINT('Ctrl Pts',(8.1,-1.68789822886868,0.202099155105557));
#12099=CARTESIAN_POINT('Ctrl Pts',(8.1,-1.67714943151225,0.403870104074094));
#12100=CARTESIAN_POINT('Ctrl Pts',(8.1,-1.67178337712185,0.50459270970527));
#12101=CARTESIAN_POINT('Ctrl Pts',(8.1,-1.66641703131627,0.605314487869832));
#12102=CARTESIAN_POINT('',(8.1,-1.7737037037037,0.));
#12103=CARTESIAN_POINT('Origin',(4.1,-1.7662962962963,0.));
#12104=CARTESIAN_POINT('',(4.1,1.70113889814581,0.));
#12105=CARTESIAN_POINT('',(4.1,-1.7662962962963,0.));
#12106=CARTESIAN_POINT('',(4.1,1.66887738702937,0.605315322680072));
#12107=CARTESIAN_POINT('Ctrl Pts',(4.1,1.66887738702937,0.605315322680072));
#12108=CARTESIAN_POINT('Ctrl Pts',(4.1,1.67424235111642,0.50466767694528));
#12109=CARTESIAN_POINT('Ctrl Pts',(4.1,1.67960699363804,0.404019058341251));
#12110=CARTESIAN_POINT('Ctrl Pts',(4.1,1.69036079691899,0.202247931921761));
#12111=CARTESIAN_POINT('Ctrl Pts',(4.1,1.6957500571643,0.101123491803998));
#12112=CARTESIAN_POINT('Ctrl Pts',(4.1,1.70113889814581,0.));
#12113=CARTESIAN_POINT('',(4.1,1.56887583540973,0.7));
#12114=CARTESIAN_POINT('Ctrl Pts',(4.1,1.56887583540973,0.7));
#12115=CARTESIAN_POINT('Ctrl Pts',(4.1,1.57679416129392,0.7));
#12116=CARTESIAN_POINT('Ctrl Pts',(4.10000107724674,1.58464912207822,0.699006028000541));
#12117=CARTESIAN_POINT('Ctrl Pts',(4.10000201939527,1.59230028572239,0.697118705459362));
#12118=CARTESIAN_POINT('Ctrl Pts',(4.10000255022779,1.59661116283941,0.696055335763773));
#12119=CARTESIAN_POINT('Ctrl Pts',(4.10000303435977,1.60085740028891,0.694707333985525));
#12120=CARTESIAN_POINT('Ctrl Pts',(4.10000334030352,1.60501217339351,0.693085708041268));
#12121=CARTESIAN_POINT('Ctrl Pts',(4.10000388718746,1.61243895913315,0.690187001388783));
#12122=CARTESIAN_POINT('Ctrl Pts',(4.10000376557609,1.61949349263125,0.686448444730844));
#12123=CARTESIAN_POINT('Ctrl Pts',(4.10000306534783,1.6260295229635,0.681951159450519));
#12124=CARTESIAN_POINT('Ctrl Pts',(4.10000267892397,1.62963645835533,0.679469313954069));
#12125=CARTESIAN_POINT('Ctrl Pts',(4.10000213012555,1.63308521926452,0.676755517937216));
#12126=CARTESIAN_POINT('Ctrl Pts',(4.1000016436875,1.63634725251217,0.673817835781739));
#12127=CARTESIAN_POINT('Ctrl Pts',(4.10000117237165,1.63950787692018,0.67097147916344));
#12128=CARTESIAN_POINT('Ctrl Pts',(4.10000075597222,1.64247408874941,0.667932078875657));
#12129=CARTESIAN_POINT('Ctrl Pts',(4.10000075698646,1.64522354659423,0.664710927554201));
#12130=CARTESIAN_POINT('Ctrl Pts',(4.1000007588733,1.65033845220459,0.658718515269377));
#12131=CARTESIAN_POINT('Ctrl Pts',(4.10000204656096,1.65470614797426,0.652098486008568));
#12132=CARTESIAN_POINT('Ctrl Pts',(4.10000248678323,1.65826650381873,0.645016049251367));
#12133=CARTESIAN_POINT('Ctrl Pts',(4.10000253228732,1.65863452415637,0.644283964909082));
#12134=CARTESIAN_POINT('Ctrl Pts',(4.10000257095464,1.65899387729575,0.643546919913709));
#12135=CARTESIAN_POINT('Ctrl Pts',(4.10000260201855,1.65934446736461,0.642805085364403));
#12136=CARTESIAN_POINT('Ctrl Pts',(4.10000290242009,1.66273482600052,0.635631222228741));
#12137=CARTESIAN_POINT('Ctrl Pts',(4.10000225562543,1.66527033938482,0.628094305374488));
#12138=CARTESIAN_POINT('Ctrl Pts',(4.10000130084992,1.66689736875237,0.62036252267401));
#12139=CARTESIAN_POINT('Ctrl Pts',(4.10000068968835,1.66793884687677,0.615413329558163));
#12140=CARTESIAN_POINT('Ctrl Pts',(4.09999999901039,1.66860722297681,0.610383627857512));
#12141=CARTESIAN_POINT('Ctrl Pts',(4.09999999630223,1.66887738567036,0.60531532268817));
#12142=CARTESIAN_POINT('',(4.1,-1.56887583540947,0.7));
#12143=CARTESIAN_POINT('',(4.1,-0.883148148148148,0.7));
#12144=CARTESIAN_POINT('',(4.1,-1.66887738702937,0.605315322680072));
#12145=CARTESIAN_POINT('Ctrl Pts',(4.09999999630223,-1.66887738567036,0.60531532268817));
#12146=CARTESIAN_POINT('Ctrl Pts',(4.10000000053001,-1.66845562780346,0.613227583070809));
#12147=CARTESIAN_POINT('Ctrl Pts',(4.10000153668442,-1.66706589531621,0.621048261667561));
#12148=CARTESIAN_POINT('Ctrl Pts',(4.10000221487211,-1.66479240287642,0.628617079688242));
#12149=CARTESIAN_POINT('Ctrl Pts',(4.10000259231836,-1.6635270876889,0.632829515245766));
#12150=CARTESIAN_POINT('Ctrl Pts',(4.10000275805793,-1.66198703315979,0.636963972243471));
#12151=CARTESIAN_POINT('Ctrl Pts',(4.10000266178038,-1.66018010017296,0.640990858692597));
#12152=CARTESIAN_POINT('Ctrl Pts',(4.10000248876893,-1.65693302887506,0.648227201990446));
#12153=CARTESIAN_POINT('Ctrl Pts',(4.10000134097948,-1.65286254930452,0.655037795911226));
#12154=CARTESIAN_POINT('Ctrl Pts',(4.100000893742,-1.6480330317196,0.661259713776781));
#12155=CARTESIAN_POINT('Ctrl Pts',(4.10000080951506,-1.647123502594,0.662431469633614));
#12156=CARTESIAN_POINT('Ctrl Pts',(4.10000075717637,-1.6461869221106,0.663582276554164));
#12157=CARTESIAN_POINT('Ctrl Pts',(4.10000075728519,-1.64522354661022,0.66471092755419));
#12158=CARTESIAN_POINT('Ctrl Pts',(4.10000075749815,-1.64333815989002,0.666919768869269));
#12159=CARTESIAN_POINT('Ctrl Pts',(4.1000009568795,-1.64135017761634,0.669043797975229));
#12160=CARTESIAN_POINT('Ctrl Pts',(4.10000122972053,-1.63926675509047,0.671079366787198));
#12161=CARTESIAN_POINT('Ctrl Pts',(4.10000197419082,-1.6335819569127,0.676633591976433));
#12162=CARTESIAN_POINT('Ctrl Pts',(4.10000313643093,-1.62725355063421,0.681469444454218));
#12163=CARTESIAN_POINT('Ctrl Pts',(4.1000035230587,-1.62044557755217,0.685533082105531));
#12164=CARTESIAN_POINT('Ctrl Pts',(4.10000376939409,-1.61610795658125,0.688122181633714));
#12165=CARTESIAN_POINT('Ctrl Pts',(4.10000375220654,-1.61157469281532,0.690397125746379));
#12166=CARTESIAN_POINT('Ctrl Pts',(4.10000346632868,-1.60688245467732,0.692334655286926));
#12167=CARTESIAN_POINT('Ctrl Pts',(4.10000302008581,-1.59955807566073,0.695359054367588));
#12168=CARTESIAN_POINT('Ctrl Pts',(4.1000019139068,-1.59193114173487,0.69752894708864));
#12169=CARTESIAN_POINT('Ctrl Pts',(4.10000102635309,-1.58414888227482,0.698774888159427));
#12170=CARTESIAN_POINT('Ctrl Pts',(4.10000045177616,-1.57911086966871,0.699581474839467));
#12171=CARTESIAN_POINT('Ctrl Pts',(4.1,-1.57400716417114,0.7));
#12172=CARTESIAN_POINT('Ctrl Pts',(4.1,-1.56887583540973,0.7));
#12173=CARTESIAN_POINT('',(4.1,-1.70113889814582,0.));
#12174=CARTESIAN_POINT('Ctrl Pts',(4.1,-1.70113889814582,0.));
#12175=CARTESIAN_POINT('Ctrl Pts',(4.1,-1.69575004793467,0.101123665001254));
#12176=CARTESIAN_POINT('Ctrl Pts',(4.1,-1.69036077845691,0.202248278345555));
#12177=CARTESIAN_POINT('Ctrl Pts',(4.1,-1.67960697517202,0.404019404791024));
#12178=CARTESIAN_POINT('Ctrl Pts',(4.1,-1.67424234188296,0.504667850166609));
#12179=CARTESIAN_POINT('Ctrl Pts',(4.1,-1.66887738702937,0.605315322680072));
#12180=CARTESIAN_POINT('',(4.1,-1.7662962962963,0.));
#12181=CARTESIAN_POINT('Origin',(1.1,-1.44962962962963,0.));
#12182=CARTESIAN_POINT('',(1.1,1.39262953588351,0.));
#12183=CARTESIAN_POINT('',(1.1,-1.44962962962963,0.));
#12184=CARTESIAN_POINT('',(1.10000000000005,1.35674377243284,0.605845626926786));
#12185=CARTESIAN_POINT('Ctrl Pts',(1.10000000000005,1.35674377243284,0.605845626926786));
#12186=CARTESIAN_POINT('Ctrl Pts',(1.10000000000005,1.36273568520883,0.504787121979256));
#12187=CARTESIAN_POINT('Ctrl Pts',(1.1,1.36872466312622,0.403727404115485));
#12188=CARTESIAN_POINT('Ctrl Pts',(1.1,1.38068651056748,0.201779555185378));
#12189=CARTESIAN_POINT('Ctrl Pts',(1.1,1.38665951284069,0.10088935150083));
#12190=CARTESIAN_POINT('Ctrl Pts',(1.1,1.39262953588351,0.));
#12191=CARTESIAN_POINT('',(1.1,1.25565664448622,0.7));
#12192=CARTESIAN_POINT('Ctrl Pts',(1.1,1.25565664448621,0.7));
#12193=CARTESIAN_POINT('Ctrl Pts',(1.1,1.26365753466764,0.700000000000001));
#12194=CARTESIAN_POINT('Ctrl Pts',(1.10000312127109,1.27160078819195,0.699008097631352));
#12195=CARTESIAN_POINT('Ctrl Pts',(1.10000579554281,1.27934333527045,0.697120485426804));
#12196=CARTESIAN_POINT('Ctrl Pts',(1.10000709386889,1.28310224676699,0.696204072889075));
#12197=CARTESIAN_POINT('Ctrl Pts',(1.10000828779753,1.28681383019745,0.695075712339665));
#12198=CARTESIAN_POINT('Ctrl Pts',(1.10000913303706,1.29046059826345,0.693742188764313));
#12199=CARTESIAN_POINT('Ctrl Pts',(1.10001087659788,1.29798315455626,0.69099139518989));
#12200=CARTESIAN_POINT('Ctrl Pts',(1.10001086910546,1.30515375246939,0.687398976275641));
#12201=CARTESIAN_POINT('Ctrl Pts',(1.10000899624477,1.31182501206943,0.683041610144935));
#12202=CARTESIAN_POINT('Ctrl Pts',(1.10000779407289,1.31610723164143,0.680244657298552));
#12203=CARTESIAN_POINT('Ctrl Pts',(1.10000585478529,1.32018349952736,0.677131483611404));
#12204=CARTESIAN_POINT('Ctrl Pts',(1.10000422180804,1.32400796947387,0.673713330684339));
#12205=CARTESIAN_POINT('Ctrl Pts',(1.10000291018178,1.3270798280974,0.670967830603965));
#12206=CARTESIAN_POINT('Ctrl Pts',(1.10000180047651,1.32997084712789,0.668041731908725));
#12207=CARTESIAN_POINT('Ctrl Pts',(1.10000182449184,1.33266034096938,0.664944387470286));
#12208=CARTESIAN_POINT('Ctrl Pts',(1.10000187074845,1.33784065079383,0.65897850512594));
#12209=CARTESIAN_POINT('Ctrl Pts',(1.10000564109429,1.34227630326151,0.652378581761819));
#12210=CARTESIAN_POINT('Ctrl Pts',(1.10000696187003,1.34590032739451,0.645305437365917));
#12211=CARTESIAN_POINT('Ctrl Pts',(1.100007110355,1.34630774940504,0.644510256482779));
#12212=CARTESIAN_POINT('Ctrl Pts',(1.10000723579819,1.34670486410349,0.643709073603569));
#12213=CARTESIAN_POINT('Ctrl Pts',(1.10000733566964,1.34709153749004,0.642902104572485));
#12214=CARTESIAN_POINT('Ctrl Pts',(1.10000822022419,1.35051627708745,0.63575483535061));
#12215=CARTESIAN_POINT('Ctrl Pts',(1.10000635568239,1.35308446649167,0.628241602461225));
#12216=CARTESIAN_POINT('Ctrl Pts',(1.10000361780323,1.35473867947858,0.620527690691125));
#12217=CARTESIAN_POINT('Ctrl Pts',(1.1000019043033,1.35577396762308,0.615699943921843));
#12218=CARTESIAN_POINT('Ctrl Pts',(1.09999998677418,1.35645041192828,0.610792997969602));
#12219=CARTESIAN_POINT('Ctrl Pts',(1.09999997754868,1.35674374570294,0.605845627052288));
#12220=CARTESIAN_POINT('',(1.1,-1.25565664448622,0.7));
#12221=CARTESIAN_POINT('',(1.1,-0.724814814814815,0.7));
#12222=CARTESIAN_POINT('',(1.10000000000005,-1.35674377243284,0.605845626926786));
#12223=CARTESIAN_POINT('Ctrl Pts',(1.09999997754868,-1.35674374570294,0.605845627052288));
#12224=CARTESIAN_POINT('Ctrl Pts',(1.09999999227748,-1.35627542940044,0.613744255356351));
#12225=CARTESIAN_POINT('Ctrl Pts',(1.1000044245081,-1.35483313756702,0.621542702113576));
#12226=CARTESIAN_POINT('Ctrl Pts',(1.10000632213307,-1.3525036790266,0.629082464357584));
#12227=CARTESIAN_POINT('Ctrl Pts',(1.1000073336739,-1.3512619466217,0.633101581650771));
#12228=CARTESIAN_POINT('Ctrl Pts',(1.10000777634458,-1.34976719347553,0.637047225321331));
#12229=CARTESIAN_POINT('Ctrl Pts',(1.10000752568741,-1.34802684471036,0.640893844816285));
#12230=CARTESIAN_POINT('Ctrl Pts',(1.10000705344834,-1.3447480208661,0.648140890909733));
#12231=CARTESIAN_POINT('Ctrl Pts',(1.10000374385205,-1.34063788586045,0.654954534019122));
#12232=CARTESIAN_POINT('Ctrl Pts',(1.10000230512149,-1.33576793982513,0.661175616324976));
#12233=CARTESIAN_POINT('Ctrl Pts',(1.10000200863552,-1.33476436716076,0.662457623989879));
#12234=CARTESIAN_POINT('Ctrl Pts',(1.10000181701501,-1.33372836971272,0.663714393476354));
#12235=CARTESIAN_POINT('Ctrl Pts',(1.10000180919237,-1.33266033853372,0.664944387472089));
#12236=CARTESIAN_POINT('Ctrl Pts',(1.10000179685332,-1.33097567746633,0.666884520904953));
#12237=CARTESIAN_POINT('Ctrl Pts',(1.10000223926429,-1.32921133126375,0.668758058859172));
#12238=CARTESIAN_POINT('Ctrl Pts',(1.10000288715521,-1.32737234926393,0.670562692084704));
#12239=CARTESIAN_POINT('Ctrl Pts',(1.10000489069569,-1.32168547392559,0.676143347135183));
#12240=CARTESIAN_POINT('Ctrl Pts',(1.10000845923633,-1.31535192007569,0.681005160308095));
#12241=CARTESIAN_POINT('Ctrl Pts',(1.1000097672184,-1.30853956043085,0.685101187995272));
#12242=CARTESIAN_POINT('Ctrl Pts',(1.10001062829021,-1.30405484229164,0.687797688271992));
#12243=CARTESIAN_POINT('Ctrl Pts',(1.10001067755751,-1.29936155475819,0.690161668140197));
#12244=CARTESIAN_POINT('Ctrl Pts',(1.10000992106221,-1.29450057597768,0.692169783635984));
#12245=CARTESIAN_POINT('Ctrl Pts',(1.10000876843985,-1.28709422081189,0.695229417764685));
#12246=CARTESIAN_POINT('Ctrl Pts',(1.100005676647,-1.27938091857402,0.69743146309387));
#12247=CARTESIAN_POINT('Ctrl Pts',(1.10000309801581,-1.2715114871423,0.698709794160748));
#12248=CARTESIAN_POINT('Ctrl Pts',(1.10000138449209,-1.26628217885177,0.699559256705032));
#12249=CARTESIAN_POINT('Ctrl Pts',(1.1,-1.26098326598685,0.700000000000001));
#12250=CARTESIAN_POINT('Ctrl Pts',(1.1,-1.25565664448621,0.7));
#12251=CARTESIAN_POINT('',(1.1,-1.39262953588351,0.));
#12252=CARTESIAN_POINT('Ctrl Pts',(1.1,-1.39262953588351,0.));
#12253=CARTESIAN_POINT('Ctrl Pts',(1.1,-1.38665944902278,0.100890429980357));
#12254=CARTESIAN_POINT('Ctrl Pts',(1.1,-1.38068638286488,0.201781712214768));
#12255=CARTESIAN_POINT('Ctrl Pts',(1.1,-1.36872453529477,0.403729561179669));
#12256=CARTESIAN_POINT('Ctrl Pts',(1.10000000000005,-1.3627356212621,0.504788200493074));
#12257=CARTESIAN_POINT('Ctrl Pts',(1.10000000000005,-1.35674377243284,0.605845626926786));
#12258=CARTESIAN_POINT('',(1.1,-1.44962962962963,0.));
#12259=CARTESIAN_POINT('Origin',(0.199725906950915,-1.4,-0.0104671912485888));
#12260=CARTESIAN_POINT('',(0.200274469199584,1.15262458915154,1.38777878078145E-17));
#12261=CARTESIAN_POINT('',(0.200274469199585,-0.7,0.));
#12262=CARTESIAN_POINT('',(0.231993417893744,1.12115139781563,0.605233595624295));
#12263=CARTESIAN_POINT('Ctrl Pts',(0.200274469199584,1.15262458915154,-5.50774703622636E-17));
#12264=CARTESIAN_POINT('Ctrl Pts',(0.210847451072758,1.1421331482829,0.201744512318911));
#12265=CARTESIAN_POINT('Ctrl Pts',(0.221420433966108,1.13164208276446,0.403489044103923));
#12266=CARTESIAN_POINT('Ctrl Pts',(0.231993417893744,1.12115139781563,0.605233595624295));
#12267=CARTESIAN_POINT('',(0.231993417893744,-1.12115139781563,0.605233595624295));
#12268=CARTESIAN_POINT('',(0.231993417893744,-0.7,0.605233595624295));
#12269=CARTESIAN_POINT('',(0.200274469199584,-1.15262458915154,1.38777878078145E-17));
#12270=CARTESIAN_POINT('Ctrl Pts',(0.231993417893744,-1.12115139781563,
0.605233595624295));
#12271=CARTESIAN_POINT('Ctrl Pts',(0.221420433966108,-1.13164208276446,
0.403489044103923));
#12272=CARTESIAN_POINT('Ctrl Pts',(0.210847451072758,-1.1421331482829,0.201744512318911));
#12273=CARTESIAN_POINT('Ctrl Pts',(0.200274469199584,-1.15262458915154,
-6.67868538251071E-17));
#12274=CARTESIAN_POINT('',(0.200274469199585,-0.7,0.));
#12275=CARTESIAN_POINT('Origin',(6.07974599480623,0.,0.));
#12276=CARTESIAN_POINT('Ctrl Pts',(8.1,-1.69866351109718,4.37041895728907E-16));
#12277=CARTESIAN_POINT('Ctrl Pts',(8.9524267631348,-1.65897367198627,1.20944032620455E-7));
#12278=CARTESIAN_POINT('Ctrl Pts',(9.80407798130771,-1.59837060538327,2.76830114922109E-8));
#12279=CARTESIAN_POINT('Ctrl Pts',(10.6537697771985,-1.52488560579501,1.03413542584124E-8));
#12280=CARTESIAN_POINT('Ctrl Pts',(10.8359404901627,-1.50913069933138,6.62336842220622E-9));
#12281=CARTESIAN_POINT('Ctrl Pts',(11.0180211259896,-1.49278349820154,3.93228299510406E-9));
#12282=CARTESIAN_POINT('Ctrl Pts',(11.2000000002909,-1.47592264092474,-3.0227174540096E-11));
#12283=CARTESIAN_POINT('Ctrl Pts',(11.2000000002909,1.47592264092474,-3.02272213335841E-11));
#12284=CARTESIAN_POINT('Ctrl Pts',(10.4240589919717,1.54781576943643,1.68591524001238E-8));
#12285=CARTESIAN_POINT('Ctrl Pts',(9.64626799696257,1.61037563220813,6.17878738288937E-8));
#12286=CARTESIAN_POINT('Ctrl Pts',(8.86753211358286,1.65747704847969,5.27022751808308E-8));
#12287=CARTESIAN_POINT('Ctrl Pts',(8.61177933690776,1.67294611604661,4.97183789310355E-8));
#12288=CARTESIAN_POINT('Ctrl Pts',(8.35592462822135,1.68674740550612,3.63007687033005E-8));
#12289=CARTESIAN_POINT('Ctrl Pts',(8.1,1.69866351109718,3.71000138306103E-16));
#12290=CARTESIAN_POINT('',(7.9,1.70758761671949,0.));
#12291=CARTESIAN_POINT('',(7.9,1.7737037037037,0.));
#12292=CARTESIAN_POINT('Ctrl Pts',(7.90000000036908,1.70758761645525,-3.06814577203155E-11));
#12293=CARTESIAN_POINT('Ctrl Pts',(7.26247716501442,1.73478515342832,3.65175246633048E-8));
#12294=CARTESIAN_POINT('Ctrl Pts',(6.624575449312,1.74993328406844,-3.04558542439636E-7));
#12295=CARTESIAN_POINT('Ctrl Pts',(5.98677261990733,1.74972113442148,-3.1918790057331E-7));
#12296=CARTESIAN_POINT('Ctrl Pts',(5.35540610719671,1.74951112565922,-3.33669628155763E-7));
#12297=CARTESIAN_POINT('Ctrl Pts',(4.72663057529054,1.73425216511322,1.21151810208783E-7));
#12298=CARTESIAN_POINT('Ctrl Pts',(4.10000000045307,1.7011388979176,-4.27317258673188E-11));
#12299=CARTESIAN_POINT('',(3.9,1.68995649764597,0.));
#12300=CARTESIAN_POINT('',(3.9,1.7662962962963,0.));
#12301=CARTESIAN_POINT('Ctrl Pts',(3.9,1.68995649764597,-1.6113354923472E-17));
#12302=CARTESIAN_POINT('Ctrl Pts',(2.96252047830716,1.63464572816558,-1.61179993858831E-17));
#12303=CARTESIAN_POINT('Ctrl Pts',(2.02971500398675,1.53866944530133,-1.61823222708931E-17));
#12304=CARTESIAN_POINT('Ctrl Pts',(1.1,1.39262953588351,-1.60717230190728E-17));
#12305=CARTESIAN_POINT('',(0.9,1.3604297237941,0.));
#12306=CARTESIAN_POINT('',(0.9,1.44962962962963,0.));
#12307=CARTESIAN_POINT('',(0.28146619846596,1.25073018526678,0.));
#12308=CARTESIAN_POINT('Ctrl Pts',(0.899999999999963,1.36042972379409,2.53412200078296E-14));
#12309=CARTESIAN_POINT('Ctrl Pts',(0.693681964344164,1.32640030945436,-1.68820282978727E-7));
#12310=CARTESIAN_POINT('Ctrl Pts',(0.487510176034459,1.28986876146525,1.95094241611213E-11));
#12311=CARTESIAN_POINT('Ctrl Pts',(0.281466198465954,1.25073018526678,9.09211941846344E-16));
#12312=CARTESIAN_POINT('Ctrl Pts',(0.28146619846596,1.25073018526678,4.90059381963448E-17));
#12313=CARTESIAN_POINT('Ctrl Pts',(0.273672142824666,1.24924968434803,-1.60851827685828E-11));
#12314=CARTESIAN_POINT('Ctrl Pts',(0.266112037439191,1.2468180315926,-2.29735811958388E-6));
#12315=CARTESIAN_POINT('Ctrl Pts',(0.258922416881026,1.24354471831116,-3.39045428380668E-6));
#12316=CARTESIAN_POINT('Ctrl Pts',(0.254316658841251,1.24144779416325,-4.09070493067818E-6));
#12317=CARTESIAN_POINT('Ctrl Pts',(0.249862973385875,1.23900427835211,-4.3601744978078E-6));
#12318=CARTESIAN_POINT('Ctrl Pts',(0.245601965247185,1.23623285256398,-4.0505643599354E-6));
#12319=CARTESIAN_POINT('Ctrl Pts',(0.238945660500109,1.23190348870705,-3.5669089987193E-6));
#12320=CARTESIAN_POINT('Ctrl Pts',(0.232836306411817,1.22682685988243,-1.47564048465526E-6));
#12321=CARTESIAN_POINT('Ctrl Pts',(0.227416445112993,1.2210931256102,-3.43092614100725E-7));
#12322=CARTESIAN_POINT('Ctrl Pts',(0.225957664245637,1.21954986437275,-3.82620891408318E-8));
#12323=CARTESIAN_POINT('Ctrl Pts',(0.224549002474426,1.21795876469157,1.76022586487844E-7));
#12324=CARTESIAN_POINT('Ctrl Pts',(0.223193686986583,1.21632111005909,2.01577349231486E-7));
#12325=CARTESIAN_POINT('Ctrl Pts',(0.221344954485829,1.21408724984631,2.36435595047204E-7));
#12326=CARTESIAN_POINT('Ctrl Pts',(0.219595448227346,1.21176677459781,-7.7718209010198E-8));
#12327=CARTESIAN_POINT('Ctrl Pts',(0.217948412504407,1.20936721934621,-5.08402878561E-7));
#12328=CARTESIAN_POINT('Ctrl Pts',(0.213467776427723,1.20283941082417,-1.68004793834142E-6));
#12329=CARTESIAN_POINT('Ctrl Pts',(0.20978887558685,1.19579640990262,-3.43350901357988E-6));
#12330=CARTESIAN_POINT('Ctrl Pts',(0.206958221875648,1.18840352636746,-3.67425174897535E-6));
#12331=CARTESIAN_POINT('Ctrl Pts',(0.206193447398199,1.18640614723908,-3.7392946395744E-6));
#12332=CARTESIAN_POINT('Ctrl Pts',(0.205490847532167,1.18438308363371,-3.7149036306613E-6));
#12333=CARTESIAN_POINT('Ctrl Pts',(0.204851940804359,1.18233735619935,-3.6037364623937E-6));
#12334=CARTESIAN_POINT('Ctrl Pts',(0.202492508448082,1.17478264548698,-3.19320484275276E-6));
#12335=CARTESIAN_POINT('Ctrl Pts',(0.201019195184615,1.16698811697394,-1.36638523817118E-6));
#12336=CARTESIAN_POINT('Ctrl Pts',(0.200491965466086,1.15911075533121,-4.28455138775697E-7));
#12337=CARTESIAN_POINT('Ctrl Pts',(0.200347608840846,1.15695391685535,-1.71647870329038E-7));
#12338=CARTESIAN_POINT('Ctrl Pts',(0.200274469313241,1.15479080601565,-7.49035961899928E-12));
#12339=CARTESIAN_POINT('Ctrl Pts',(0.200274469199584,1.15262458915154,9.10729824887824E-18));
#12340=CARTESIAN_POINT('',(2.01407162049393E-18,1.15316892111334,2.77409355997279E-17));
#12341=CARTESIAN_POINT('',(0.,-1.4,0.));
#12342=CARTESIAN_POINT('',(0.243580684154574,1.44748675362873,2.77555756156289E-17));
#12343=CARTESIAN_POINT('Ctrl Pts',(0.243580684154575,1.44748675362873,-1.56125112837913E-16));
#12344=CARTESIAN_POINT('Ctrl Pts',(0.226022619058538,1.44415189332774,-6.74769223000006E-12));
#12345=CARTESIAN_POINT('Ctrl Pts',(0.208837776424359,1.43922483814223,-1.83343972289099E-6));
#12346=CARTESIAN_POINT('Ctrl Pts',(0.192216855517481,1.43283671850359,-2.37047811876899E-6));
#12347=CARTESIAN_POINT('Ctrl Pts',(0.175448307189507,1.42639185943196,-2.91228650265529E-6));
#12348=CARTESIAN_POINT('Ctrl Pts',(0.15925228528901,1.41845922211561,-2.09168970691363E-6));
#12349=CARTESIAN_POINT('Ctrl Pts',(0.143842215871583,1.4091253227419,-1.20497646612983E-7));
#12350=CARTESIAN_POINT('Ctrl Pts',(0.141154971457358,1.40749765525544,2.23243494969264E-7));
#12351=CARTESIAN_POINT('Ctrl Pts',(0.138491701959641,1.40582727297256,5.92673833856784E-7));
#12352=CARTESIAN_POINT('Ctrl Pts',(0.135853645420207,1.40411450883245,9.74556207071009E-7));
#12353=CARTESIAN_POINT('Ctrl Pts',(0.120686164410185,1.39426698768136,3.17018528370531E-6));
#12354=CARTESIAN_POINT('Ctrl Pts',(0.106484701177391,1.38310949089167,6.09567884445769E-6));
#12355=CARTESIAN_POINT('Ctrl Pts',(0.0934509959242968,1.37075049507673,
5.10227143121889E-6));
#12356=CARTESIAN_POINT('Ctrl Pts',(0.0918301157095608,1.36921352217444,
4.97873062758527E-6));
#12357=CARTESIAN_POINT('Ctrl Pts',(0.0902273306836925,1.36765791150105,
4.78983320752683E-6));
#12358=CARTESIAN_POINT('Ctrl Pts',(0.0886430622088043,1.36608382581751,
4.52250464763623E-6));
#12359=CARTESIAN_POINT('Ctrl Pts',(0.0755027622673366,1.35302798437193,
2.30521792157715E-6));
#12360=CARTESIAN_POINT('Ctrl Pts',(0.0636322991078783,1.33870385142449,
-4.95851449924696E-6));
#12361=CARTESIAN_POINT('Ctrl Pts',(0.0531272107863483,1.3233265665666,-1.07771754856876E-5));
#12362=CARTESIAN_POINT('Ctrl Pts',(0.0429100363670196,1.3083707283404,-1.64363639061758E-5));
#12363=CARTESIAN_POINT('Ctrl Pts',(0.0340657397255946,1.29253754778979,
-2.07072841115287E-5));
#12364=CARTESIAN_POINT('Ctrl Pts',(0.026663056477648,1.27603964904139,-2.15377272154938E-5));
#12365=CARTESIAN_POINT('Ctrl Pts',(0.0217318501145713,1.26504977678014,
-2.20909166714363E-5));
#12366=CARTESIAN_POINT('Ctrl Pts',(0.0174411483101006,1.25376411673155,
-2.12025196266096E-5));
#12367=CARTESIAN_POINT('Ctrl Pts',(0.01382286588119,1.24224013948332,-1.91534441809703E-5));
#12368=CARTESIAN_POINT('Ctrl Pts',(0.00842668188255806,1.22505366970124,
-1.60975223868617E-5));
#12369=CARTESIAN_POINT('Ctrl Pts',(0.00456091079961661,1.20745571355567,
-1.03588883906395E-5));
#12370=CARTESIAN_POINT('Ctrl Pts',(0.0023097402764219,1.18964331095195,
-5.71664032024866E-6));
#12371=CARTESIAN_POINT('Ctrl Pts',(0.00078319128522165,1.17756448131848,
-2.56866950429304E-6));
#12372=CARTESIAN_POINT('Ctrl Pts',(2.50028438421117E-9,1.16538650529032,
-1.91718613723104E-10));
#12373=CARTESIAN_POINT('Ctrl Pts',(-1.21430643318376E-17,1.15316892111333,
5.20417042793042E-18));
#12374=CARTESIAN_POINT('',(11.7295909468525,1.62672708026858,5.55111512312578E-17));
#12375=CARTESIAN_POINT('Ctrl Pts',(0.243580684154574,1.44748675362873,0.));
#12376=CARTESIAN_POINT('Ctrl Pts',(4.07225077172054,2.17467835246083,0.));
#12377=CARTESIAN_POINT('Ctrl Pts',(7.90092085928651,2.00057770191527,0.));
#12378=CARTESIAN_POINT('Ctrl Pts',(11.7295909468525,1.62672708026858,0.));
#12379=CARTESIAN_POINT('',(12.,1.32855945177638,-4.17473993839455E-17));
#12380=CARTESIAN_POINT('Ctrl Pts',(12.,1.32855945177638,2.42861286636753E-16));
#12381=CARTESIAN_POINT('Ctrl Pts',(11.9999999991614,1.34640852075174,-1.28298622986823E-11));
#12382=CARTESIAN_POINT('Ctrl Pts',(11.9983618543561,1.36418409382152,-2.22383001277967E-6));
#12383=CARTESIAN_POINT('Ctrl Pts',(11.9951861391139,1.38167870884165,-3.43465861540838E-6));
#12384=CARTESIAN_POINT('Ctrl Pts',(11.9919727904737,1.39938064150867,-4.65983598400874E-6));
#12385=CARTESIAN_POINT('Ctrl Pts',(11.9871848331028,1.41679645887758,-4.78742071954366E-6));
#12386=CARTESIAN_POINT('Ctrl Pts',(11.9808755917115,1.43370272794343,-3.5739118077222E-6));
#12387=CARTESIAN_POINT('Ctrl Pts',(11.9797611226834,1.43668906371449,-3.35955670324834E-6));
#12388=CARTESIAN_POINT('Ctrl Pts',(11.9785990681726,1.43965944485564,-3.11247275469786E-6));
#12389=CARTESIAN_POINT('Ctrl Pts',(11.9773895732386,1.44261255525912,-2.84353511336506E-6));
#12390=CARTESIAN_POINT('Ctrl Pts',(11.9705369081732,1.45934406518776,-1.31980853313606E-6));
#12391=CARTESIAN_POINT('Ctrl Pts',(11.9622259501015,1.47537448669426,1.24030492427686E-6));
#12392=CARTESIAN_POINT('Ctrl Pts',(11.9525330320198,1.49048867890869,8.79804099270529E-7));
#12393=CARTESIAN_POINT('Ctrl Pts',(11.9492586078121,1.49559449703792,7.58021100761347E-7));
#12394=CARTESIAN_POINT('Ctrl Pts',(11.9458260650319,1.50059560584699,2.73671093112169E-7));
#12395=CARTESIAN_POINT('Ctrl Pts',(11.9422371454499,1.50548309160802,-8.21070286398525E-7));
#12396=CARTESIAN_POINT('Ctrl Pts',(11.9335276940755,1.51734385321214,-3.47774636801117E-6));
#12397=CARTESIAN_POINT('Ctrl Pts',(11.923898315087,1.52853671512454,-9.61160164537397E-6));
#12398=CARTESIAN_POINT('Ctrl Pts',(11.9134480753511,1.53899918600446,-1.54908303532852E-5));
#12399=CARTESIAN_POINT('Ctrl Pts',(11.9006414429521,1.55182080751067,-2.26957483986032E-5));
#12400=CARTESIAN_POINT('Ctrl Pts',(11.8867118754531,1.56343792791748,-2.93307907620841E-5));
#12401=CARTESIAN_POINT('Ctrl Pts',(11.8718669715436,1.57375979462261,-3.2097080434168E-5));
#12402=CARTESIAN_POINT('Ctrl Pts',(11.8583226919989,1.58317731924447,-3.46210038525051E-5));
#12403=CARTESIAN_POINT('Ctrl Pts',(11.84401509256,1.59151672629289,-3.39892197405707E-5));
#12404=CARTESIAN_POINT('Ctrl Pts',(11.8290799708805,1.59867837245092,-3.04453078860132E-5));
#12405=CARTESIAN_POINT('Ctrl Pts',(11.8128282236205,1.60647136308226,-2.65889777530425E-5));
#12406=CARTESIAN_POINT('Ctrl Pts',(11.7959622791259,1.61280865470064,-1.93051308245346E-5));
#12407=CARTESIAN_POINT('Ctrl Pts',(11.7786680578171,1.61758555622507,-1.24065785496921E-5));
#12408=CARTESIAN_POINT('Ctrl Pts',(11.7626326571209,1.62201475420184,-6.0101616208217E-6));
#12409=CARTESIAN_POINT('Ctrl Pts',(11.7462278952123,1.62510256303752,-1.15598952599692E-10));
#12410=CARTESIAN_POINT('Ctrl Pts',(11.7295909468525,1.62672708026857,-1.01481323344643E-16));
#12411=CARTESIAN_POINT('',(12.,-1.32855945177638,-2.7831599589297E-17));
#12412=CARTESIAN_POINT('',(12.,1.6,0.));
#12413=CARTESIAN_POINT('',(11.7295909468525,-1.62672708026858,-2.77555756156289E-17));
#12414=CARTESIAN_POINT('Ctrl Pts',(11.7295909468525,-1.62672708026858,2.76688394418301E-16));
#12415=CARTESIAN_POINT('Ctrl Pts',(11.7473502233519,-1.62499297457843,3.63491969896433E-13));
#12416=CARTESIAN_POINT('Ctrl Pts',(11.7648769397846,-1.62163540491215,-2.46542030701863E-6));
#12417=CARTESIAN_POINT('Ctrl Pts',(11.7819744899096,-1.61677476461769,-3.87870576098494E-6));
#12418=CARTESIAN_POINT('Ctrl Pts',(11.799277951102,-1.61185558613358,-5.30901184740094E-6));
#12419=CARTESIAN_POINT('Ctrl Pts',(11.8161433440738,-1.60539638769883,-5.61072687595782E-6));
#12420=CARTESIAN_POINT('Ctrl Pts',(11.8323535184498,-1.59747214364331,-4.43708131311936E-6));
#12421=CARTESIAN_POINT('Ctrl Pts',(11.8351986841263,-1.59608130189932,-4.23108623901291E-6));
#12422=CARTESIAN_POINT('Ctrl Pts',(11.8380235988884,-1.59464521634493,-3.98890160078043E-6));
#12423=CARTESIAN_POINT('Ctrl Pts',(11.8408269920241,-1.59316415515964,-3.72087260345577E-6));
#12424=CARTESIAN_POINT('Ctrl Pts',(11.8568148563263,-1.58471760338924,-2.19229240409177E-6));
#12425=CARTESIAN_POINT('Ctrl Pts',(11.8719627312575,-1.57488689795395,5.08047814114288E-7));
#12426=CARTESIAN_POINT('Ctrl Pts',(11.8860639991294,-1.56376935451958,3.7910357452838E-7));
#12427=CARTESIAN_POINT('Ctrl Pts',(11.8908390360804,-1.5600046802233,3.35439876042474E-7));
#12428=CARTESIAN_POINT('Ctrl Pts',(11.8954938739134,-1.55609205312677,-6.31409548673105E-8));
#12429=CARTESIAN_POINT('Ctrl Pts',(11.9000197537765,-1.55203410647271,-1.07033715310124E-6));
#12430=CARTESIAN_POINT('Ctrl Pts',(11.9109521284419,-1.54223203603875,-3.50324446252274E-6));
#12431=CARTESIAN_POINT('Ctrl Pts',(11.9211333865357,-1.53158293117673,-9.37257606292525E-6));
#12432=CARTESIAN_POINT('Ctrl Pts',(11.9305114837192,-1.52019095639426,-1.50133174764804E-5));
#12433=CARTESIAN_POINT('Ctrl Pts',(11.9420285825687,-1.50620064502377,-2.19406264148308E-5));
#12434=CARTESIAN_POINT('Ctrl Pts',(11.9522379825693,-1.49120969914507,-2.8349487615449E-5));
#12435=CARTESIAN_POINT('Ctrl Pts',(11.9610699533786,-1.47543375940277,-3.10096306454085E-5));
#12436=CARTESIAN_POINT('Ctrl Pts',(11.9691383866925,-1.46102167397773,-3.34398002084833E-5));
#12437=CARTESIAN_POINT('Ctrl Pts',(11.976057247492,-1.44595309822982,-3.28127654573608E-5));
#12438=CARTESIAN_POINT('Ctrl Pts',(11.9817405815488,-1.43037347552767,-2.93737351251587E-5));
#12439=CARTESIAN_POINT('Ctrl Pts',(11.9879190063177,-1.41343666945002,-2.56351214921306E-5));
#12440=CARTESIAN_POINT('Ctrl Pts',(11.9925890154887,-1.39602986621001,-1.86015881889918E-5));
#12441=CARTESIAN_POINT('Ctrl Pts',(11.9956646601292,-1.37834843064327,-1.1951505214167E-5));
#12442=CARTESIAN_POINT('Ctrl Pts',(11.9985188379205,-1.36194017591583,-5.78027239782095E-6));
#12443=CARTESIAN_POINT('Ctrl Pts',(11.9999999979315,-1.34529424449622,-1.63143103698095E-10));
#12444=CARTESIAN_POINT('Ctrl Pts',(12.,-1.32855945177638,6.07153216591882E-17));
#12445=CARTESIAN_POINT('',(0.243580684154574,-1.44748675362873,-2.77555756156289E-17));
#12446=CARTESIAN_POINT('Ctrl Pts',(11.7295909468525,-1.62672708026858,0.));
#12447=CARTESIAN_POINT('Ctrl Pts',(7.90092085928651,-2.00057770191527,0.));
#12448=CARTESIAN_POINT('Ctrl Pts',(4.07225077172054,-2.17467835246083,0.));
#12449=CARTESIAN_POINT('Ctrl Pts',(0.243580684154574,-1.44748675362873,
0.));
#12450=CARTESIAN_POINT('',(-2.01407162049393E-18,-1.15316892111334,-2.77409355997279E-17));
#12451=CARTESIAN_POINT('Ctrl Pts',(-1.45716771982052E-16,-1.15316892111333,
-8.67361737988404E-17));
#12452=CARTESIAN_POINT('Ctrl Pts',(1.25998894435939E-9,-1.17105087373522,
-1.90287520688926E-11));
#12453=CARTESIAN_POINT('Ctrl Pts',(0.00163339464743996,-1.18886359576077,
-1.42965894531121E-6));
#12454=CARTESIAN_POINT('Ctrl Pts',(0.00480727841906161,-1.20639511031145,
-1.64093682142839E-6));
#12455=CARTESIAN_POINT('Ctrl Pts',(0.00800796397580062,-1.22407466931478,
-1.8539988284852E-6));
#12456=CARTESIAN_POINT('Ctrl Pts',(0.0127756311263789,-1.24146980201313,
-7.66483898132055E-7));
#12457=CARTESIAN_POINT('Ctrl Pts',(0.0190655400899108,-1.25835467436912,
1.24978183846727E-6));
#12458=CARTESIAN_POINT('Ctrl Pts',(0.0201762582672253,-1.26133632875492,
1.60582880463507E-6));
#12459=CARTESIAN_POINT('Ctrl Pts',(0.0213345630164365,-1.2643020159517,
1.98173645466097E-6));
#12460=CARTESIAN_POINT('Ctrl Pts',(0.022540357064946,-1.26725040777374,
2.36324320385681E-6));
#12461=CARTESIAN_POINT('Ctrl Pts',(0.0293845669280623,-1.28398578013164,
4.5287143794027E-6));
#12462=CARTESIAN_POINT('Ctrl Pts',(0.0376942987862453,-1.30001720705818,
7.20349268724091E-6));
#12463=CARTESIAN_POINT('Ctrl Pts',(0.0474014865253391,-1.31512615530125,
5.82569015349308E-6));
#12464=CARTESIAN_POINT('Ctrl Pts',(0.0485928463173857,-1.31698047129067,
5.65659292531477E-6));
#12465=CARTESIAN_POINT('Ctrl Pts',(0.049805315173965,-1.3188208685659,5.4220814195758E-6));
#12466=CARTESIAN_POINT('Ctrl Pts',(0.0510388164126442,-1.32064691964073,
5.10992468070797E-6));
#12467=CARTESIAN_POINT('Ctrl Pts',(0.0614399911345998,-1.33604461498541,
2.47774509321499E-6));
#12468=CARTESIAN_POINT('Ctrl Pts',(0.0733332132114129,-1.35042574344132,
-5.3152380038924E-6));
#12469=CARTESIAN_POINT('Ctrl Pts',(0.0865238753361435,-1.36365441213776,
-1.1550981620978E-5));
#12470=CARTESIAN_POINT('Ctrl Pts',(0.0993129767592984,-1.37648036310613,
-1.75968917362996E-5));
#12471=CARTESIAN_POINT('Ctrl Pts',(0.113220041589059,-1.38812080263946,
-2.21381304374214E-5));
#12472=CARTESIAN_POINT('Ctrl Pts',(0.128049501721596,-1.3984678073416,-2.30260298918279E-5));
#12473=CARTESIAN_POINT('Ctrl Pts',(0.137898881094142,-1.40534004502052,
-2.36157518704412E-5));
#12474=CARTESIAN_POINT('Ctrl Pts',(0.148156110210342,-1.41164106947418,
-2.26770903305374E-5));
#12475=CARTESIAN_POINT('Ctrl Pts',(0.158771208267938,-1.41732893485082,
-2.05010084084185E-5));
#12476=CARTESIAN_POINT('Ctrl Pts',(0.174640735071984,-1.42583226958806,
-1.72477751171679E-5));
#12477=CARTESIAN_POINT('Ctrl Pts',(0.191199787345415,-1.4329086754137,-1.11085100333009E-5));
#12478=CARTESIAN_POINT('Ctrl Pts',(0.208270835533445,-1.43843835369108,
-6.12965879291162E-6));
#12479=CARTESIAN_POINT('Ctrl Pts',(0.219822542278978,-1.44218019901621,
-2.76054936125183E-6));
#12480=CARTESIAN_POINT('Ctrl Pts',(0.231609382520684,-1.4452130041726,-1.10646384277296E-10));
#12481=CARTESIAN_POINT('Ctrl Pts',(0.243580684154575,-1.44748675362873,
-8.67361737988404E-18));
#12482=CARTESIAN_POINT('',(0.,-1.4,0.));
#12483=CARTESIAN_POINT('',(0.28146619846596,-1.25073018526678,-1.38777878078145E-17));
#12484=CARTESIAN_POINT('Ctrl Pts',(0.200274469199584,-1.15262458915154,
-4.38017677684144E-17));
#12485=CARTESIAN_POINT('Ctrl Pts',(0.200274469606231,-1.16056122076396,
-2.67994619525583E-11));
#12486=CARTESIAN_POINT('Ctrl Pts',(0.201251993787099,-1.16844573575355,
-2.06906772440415E-6));
#12487=CARTESIAN_POINT('Ctrl Pts',(0.203125250303271,-1.17612349127761,
-3.03593176598444E-6));
#12488=CARTESIAN_POINT('Ctrl Pts',(0.204328175564463,-1.18105381768481,
-3.65681052429326E-6));
#12489=CARTESIAN_POINT('Ctrl Pts',(0.205901645655995,-1.18589907428975,
-3.87486521964464E-6));
#12490=CARTESIAN_POINT('Ctrl Pts',(0.207834893326199,-1.19061551412018,
-3.56660141708203E-6));
#12491=CARTESIAN_POINT('Ctrl Pts',(0.210845733886816,-1.19796089907112,
-3.08651126907409E-6));
#12492=CARTESIAN_POINT('Ctrl Pts',(0.214691665920849,-1.20490884791767,
-1.13290501265697E-6));
#12493=CARTESIAN_POINT('Ctrl Pts',(0.219311372289421,-1.21130241743461,
-1.88024479619773E-7));
#12494=CARTESIAN_POINT('Ctrl Pts',(0.220549822002528,-1.21301640393121,
6.52788543367939E-8));
#12495=CARTESIAN_POINT('Ctrl Pts',(0.22184414018537,-1.21469042595737,2.26073670777299E-7));
#12496=CARTESIAN_POINT('Ctrl Pts',(0.223193686901845,-1.21632111014354,
1.99977909429435E-7));
#12497=CARTESIAN_POINT('Ctrl Pts',(0.225054776233359,-1.21856990146355,
1.63990609064731E-7));
#12498=CARTESIAN_POINT('Ctrl Pts',(0.227020882846909,-1.2207363067163,-2.2494482424301E-7));
#12499=CARTESIAN_POINT('Ctrl Pts',(0.229085096241527,-1.22281561536867,
-7.25033596408456E-7));
#12500=CARTESIAN_POINT('Ctrl Pts',(0.234663732853057,-1.22843504764494,
-2.07654770860772E-6));
#12501=CARTESIAN_POINT('Ctrl Pts',(0.240898147116973,-1.23336261820331,
-3.93931381885212E-6));
#12502=CARTESIAN_POINT('Ctrl Pts',(0.247634917667946,-1.2375211924479,-4.15647360184107E-6));
#12503=CARTESIAN_POINT('Ctrl Pts',(0.24944409362824,-1.23863798757926,-4.21479238469909E-6));
#12504=CARTESIAN_POINT('Ctrl Pts',(0.251289686356224,-1.23969909864123,
-4.17584617698396E-6));
#12505=CARTESIAN_POINT('Ctrl Pts',(0.253169062337335,-1.24070249413235,
-4.04352721072409E-6));
#12506=CARTESIAN_POINT('Ctrl Pts',(0.260147540238377,-1.24442829106235,
-3.55220190316667E-6));
#12507=CARTESIAN_POINT('Ctrl Pts',(0.267526846148503,-1.24732811138375,
-1.51439637010182E-6));
#12508=CARTESIAN_POINT('Ctrl Pts',(0.275164162321015,-1.24931347733136,
-4.73394739174148E-7));
#12509=CARTESIAN_POINT('Ctrl Pts',(0.277246452424842,-1.24985478107889,
-1.89568936341825E-7));
#12510=CARTESIAN_POINT('Ctrl Pts',(0.27934803608603,-1.25032783487679,-4.20368826828312E-12));
#12511=CARTESIAN_POINT('Ctrl Pts',(0.28146619846596,-1.25073018526678,1.2793585635329E-17));
#12512=CARTESIAN_POINT('',(0.9,-1.3604297237941,0.));
#12513=CARTESIAN_POINT('Ctrl Pts',(0.281466198465954,-1.25073018526678,
9.63150999927498E-16));
#12514=CARTESIAN_POINT('Ctrl Pts',(0.487510152792939,-1.28986875705046,
1.95065110193295E-11));
#12515=CARTESIAN_POINT('Ctrl Pts',(0.693681940810289,-1.32640030557063,
-1.68784634270162E-7));
#12516=CARTESIAN_POINT('Ctrl Pts',(0.899999999999961,-1.36042972379409,
2.52314774976951E-14));
#12517=CARTESIAN_POINT('',(0.9,1.44962962962963,0.));
#12518=CARTESIAN_POINT('',(3.9,-1.68995649764597,0.));
#12519=CARTESIAN_POINT('Ctrl Pts',(1.1,-1.39262953588351,-2.05019623674552E-17));
#12520=CARTESIAN_POINT('Ctrl Pts',(2.02971449277185,-1.53866936499954,-2.04062575199768E-17));
#12521=CARTESIAN_POINT('Ctrl Pts',(2.96251993741879,-1.63464569625347,-2.05230086706555E-17));
#12522=CARTESIAN_POINT('Ctrl Pts',(3.9,-1.68995649764597,-2.05203881127908E-17));
#12523=CARTESIAN_POINT('',(3.9,1.7662962962963,0.));
#12524=CARTESIAN_POINT('',(7.9,-1.70758761671949,0.));
#12525=CARTESIAN_POINT('Ctrl Pts',(4.10000000045307,-1.7011388979176,-4.27317380631109E-11));
#12526=CARTESIAN_POINT('Ctrl Pts',(4.72643887491804,-1.7342420350347,1.20853286712337E-7));
#12527=CARTESIAN_POINT('Ctrl Pts',(5.35502164560988,-1.74950180199062,-3.33551248611792E-7));
#12528=CARTESIAN_POINT('Ctrl Pts',(5.98619394951577,-1.74972093772735,-3.1920111515717E-7));
#12529=CARTESIAN_POINT('Ctrl Pts',(6.62418968669829,-1.74994244248134,-3.0469584628258E-7));
#12530=CARTESIAN_POINT('Ctrl Pts',(7.26228442347589,-1.73479337602516,3.6583895104054E-8));
#12531=CARTESIAN_POINT('Ctrl Pts',(7.90000000036908,-1.70758761645525,-3.06816097140251E-11));
#12532=CARTESIAN_POINT('',(7.9,1.7737037037037,0.));
#12533=CARTESIAN_POINT('',(11.4,-1.45718524058191,0.));
#12534=CARTESIAN_POINT('',(11.7095901160181,-1.42740242188993,1.38777878078145E-17));
#12535=CARTESIAN_POINT('Ctrl Pts',(11.4000000008084,-1.45718524050535,1.02728155843002E-16));
#12536=CARTESIAN_POINT('Ctrl Pts',(11.5032315878449,-1.44740895658952,-1.62414911853346E-10));
#12537=CARTESIAN_POINT('Ctrl Pts',(11.6064290066394,-1.43747657129068,3.17212713797596E-13));
#12538=CARTESIAN_POINT('Ctrl Pts',(11.7095901160181,-1.42740242188993,-1.31135713082882E-16));
#12539=CARTESIAN_POINT('',(11.7997255308004,-1.32801330383774,0.));
#12540=CARTESIAN_POINT('Ctrl Pts',(11.7095901160181,-1.42740242188993,-9.19403442267708E-17));
#12541=CARTESIAN_POINT('Ctrl Pts',(11.7174875668098,-1.42663119997609,-1.06723531187443E-12));
#12542=CARTESIAN_POINT('Ctrl Pts',(11.7252481284326,-1.42489860698852,-1.31351091787008E-6));
#12543=CARTESIAN_POINT('Ctrl Pts',(11.7327147629935,-1.4222933789697,-1.57347087725304E-6));
#12544=CARTESIAN_POINT('Ctrl Pts',(11.7375034508718,-1.42062252930751,-1.7401948673154E-6));
#12545=CARTESIAN_POINT('Ctrl Pts',(11.742171336984,-1.41859157258352,-1.52962160850981E-6));
#12546=CARTESIAN_POINT('Ctrl Pts',(11.7466731630754,-1.4162133745499,-1.06822103866601E-6));
#12547=CARTESIAN_POINT('Ctrl Pts',(11.7538080604269,-1.41244419322064,-3.36952074275293E-7));
#12548=CARTESIAN_POINT('Ctrl Pts',(11.7604421378066,-1.40785009750528,1.23525126371337E-6));
#12549=CARTESIAN_POINT('Ctrl Pts',(11.7664060685299,-1.40250292630552,-7.85770423176645E-8));
#12550=CARTESIAN_POINT('Ctrl Pts',(11.7700505374369,-1.39923534992309,-8.81437879006801E-7));
#12551=CARTESIAN_POINT('Ctrl Pts',(11.7734443324447,-1.39568546479044,-2.84121358692309E-6));
#12552=CARTESIAN_POINT('Ctrl Pts',(11.7765701913309,-1.39188797822873,-4.73246891796253E-6));
#12553=CARTESIAN_POINT('Ctrl Pts',(11.7816218974528,-1.38575085342217,-7.78893003218221E-6));
#12554=CARTESIAN_POINT('Ctrl Pts',(11.7859196635778,-1.3790373064984,-1.04294718165207E-5));
#12555=CARTESIAN_POINT('Ctrl Pts',(11.7894058487846,-1.37190723377291,-1.0649753115785E-5));
#12556=CARTESIAN_POINT('Ctrl Pts',(11.7909886780302,-1.36866997385604,-1.07497672177443E-5));
#12557=CARTESIAN_POINT('Ctrl Pts',(11.7924036476919,-1.36534638272796,-1.04045251440782E-5));
#12558=CARTESIAN_POINT('Ctrl Pts',(11.7936422141268,-1.36194984358789,-9.67400732978531E-6));
#12559=CARTESIAN_POINT('Ctrl Pts',(11.7963517531347,-1.35451943450186,-8.0758964348484E-6));
#12560=CARTESIAN_POINT('Ctrl Pts',(11.7981920551596,-1.34681816044402,-4.45435127417515E-6));
#12561=CARTESIAN_POINT('Ctrl Pts',(11.7990923524223,-1.33899256731255,-1.99131993767782E-6));
#12562=CARTESIAN_POINT('Ctrl Pts',(11.7995108157868,-1.33535518645399,-8.46488755312323E-7));
#12563=CARTESIAN_POINT('Ctrl Pts',(11.7997255306472,-1.33169069466208,-1.20180646731727E-11));
#12564=CARTESIAN_POINT('Ctrl Pts',(11.7997255308004,-1.32801330383774,1.56125112837913E-17));
#12565=CARTESIAN_POINT('',(11.7997255308004,1.32801330383774,-1.38777878078145E-17));
#12566=CARTESIAN_POINT('',(11.7997255308004,0.8,0.));
#12567=CARTESIAN_POINT('',(11.7095901160181,1.42740242188993,1.38777878078145E-17));
#12568=CARTESIAN_POINT('Ctrl Pts',(11.7997255308004,1.32801330383774,3.29597460435593E-17));
#12569=CARTESIAN_POINT('Ctrl Pts',(11.7997255306701,1.33594993357028,-3.19998942079111E-12));
#12570=CARTESIAN_POINT('Ctrl Pts',(11.7987557313351,1.34384388324515,-1.1738056914779E-6));
#12571=CARTESIAN_POINT('Ctrl Pts',(11.7968890528831,1.35153020534854,-1.35082478761126E-6));
#12572=CARTESIAN_POINT('Ctrl Pts',(11.7956902940742,1.35646627043222,-1.46450435604653E-6));
#12573=CARTESIAN_POINT('Ctrl Pts',(11.7941204989552,1.36131691981906,-1.21679535622301E-6));
#12574=CARTESIAN_POINT('Ctrl Pts',(11.7921880664813,1.36603565236267,-7.51718013047842E-7));
#12575=CARTESIAN_POINT('Ctrl Pts',(11.7891321441143,1.37349779167052,-1.62510435539431E-8));
#12576=CARTESIAN_POINT('Ctrl Pts',(11.7852081688769,1.38054242009704,1.47305143123643E-6));
#12577=CARTESIAN_POINT('Ctrl Pts',(11.7804707482717,1.38699431162271,4.31295153147674E-8));
#12578=CARTESIAN_POINT('Ctrl Pts',(11.7775673564694,1.39094843993989,-8.33217322910001E-7));
#12579=CARTESIAN_POINT('Ctrl Pts',(11.774357304366,1.39467961749964,-2.88177890715362E-6));
#12580=CARTESIAN_POINT('Ctrl Pts',(11.7708736118052,1.39816709864095,-4.85419454747415E-6));
#12581=CARTESIAN_POINT('Ctrl Pts',(11.7652557092992,1.40379111072049,-8.03496856102318E-6));
#12582=CARTESIAN_POINT('Ctrl Pts',(11.7589908599241,1.40872063947841,-1.07717451179728E-5));
#12583=CARTESIAN_POINT('Ctrl Pts',(11.7522324303862,1.41288246393566,-1.10093962897399E-5));
#12584=CARTESIAN_POINT('Ctrl Pts',(11.7491699691574,1.41476832010531,-1.11170836593312E-5));
#12585=CARTESIAN_POINT('Ctrl Pts',(11.7460056456443,1.41649603445901,-1.07652933077188E-5));
#12586=CARTESIAN_POINT('Ctrl Pts',(11.7427518690514,1.41805582819498,-1.00150721194158E-5));
#12587=CARTESIAN_POINT('Ctrl Pts',(11.7356218627913,1.421473806899,-8.37111113549047E-6));
#12588=CARTESIAN_POINT('Ctrl Pts',(11.7281378774234,1.42405291512428,-4.62166314666036E-6));
#12589=CARTESIAN_POINT('Ctrl Pts',(11.7204387731059,1.42570834923663,-2.06587013620581E-6));
#12590=CARTESIAN_POINT('Ctrl Pts',(11.7168648812537,1.42647679479109,-8.79481766934018E-7));
#12591=CARTESIAN_POINT('Ctrl Pts',(11.7132443218769,1.42704557200794,-8.45784208685192E-12));
#12592=CARTESIAN_POINT('Ctrl Pts',(11.7095901160181,1.42740242188993,2.53703308361608E-17));
#12593=CARTESIAN_POINT('',(11.4,1.45718524058191,0.));
#12594=CARTESIAN_POINT('Ctrl Pts',(11.7095901160181,1.42740242188993,-2.09644042577228E-16));
#12595=CARTESIAN_POINT('Ctrl Pts',(11.6064290073882,1.43747657121756,3.16925904777201E-13));
#12596=CARTESIAN_POINT('Ctrl Pts',(11.5032315885351,1.44740895652415,-1.62368751268212E-10));
#12597=CARTESIAN_POINT('Ctrl Pts',(11.4000000008083,1.45718524050537,-7.57963810214684E-17));
#12598=CARTESIAN_POINT('',(11.4,-1.53779953703704,0.));
#12599=CARTESIAN_POINT('Origin',(10.,0.,0.));
#12600=CARTESIAN_POINT('',(9.6,-4.89858719658942E-17,0.7));
#12601=CARTESIAN_POINT('Origin',(10.,0.,0.7));
#12602=CARTESIAN_POINT('',(9.6,-4.89858719658942E-17,0.));
#12603=CARTESIAN_POINT('Origin',(2.,0.,0.));
#12604=CARTESIAN_POINT('',(1.6,-4.89858719658941E-17,0.7));
#12605=CARTESIAN_POINT('Origin',(2.,0.,0.7));
#12606=CARTESIAN_POINT('',(1.6,-4.89858719658941E-17,0.));
#12607=CARTESIAN_POINT('Origin',(11.4,-1.53779953703704,0.));
#12608=CARTESIAN_POINT('',(11.4,-1.4227102204299,0.605660349289938));
#12609=CARTESIAN_POINT('Ctrl Pts',(11.4,-1.45718524058191,0.));
#12610=CARTESIAN_POINT('Ctrl Pts',(11.4,-1.45144762186897,0.100853500740053));
#12611=CARTESIAN_POINT('Ctrl Pts',(11.4,-1.44570843451869,0.201707502489292));
#12612=CARTESIAN_POINT('Ctrl Pts',(11.4,-1.43421679834229,0.403593890565801));
#12613=CARTESIAN_POINT('Ctrl Pts',(11.4,-1.42846427656079,0.504627461196798));
#12614=CARTESIAN_POINT('Ctrl Pts',(11.4,-1.4227102204299,0.605660349289938));
#12615=CARTESIAN_POINT('',(11.4,1.4227102204299,0.605660349289938));
#12616=CARTESIAN_POINT('Ctrl Pts',(11.4,1.4227102204299,0.605660349289938));
#12617=CARTESIAN_POINT('Ctrl Pts',(11.4,1.42846501637408,0.504614471147338));
#12618=CARTESIAN_POINT('Ctrl Pts',(11.4,1.43421827757761,0.403567910233218));
#12619=CARTESIAN_POINT('Ctrl Pts',(11.4,1.44570991295315,0.201681522149997));
#12620=CARTESIAN_POINT('Ctrl Pts',(11.4,1.45144836088146,0.100840510682596));
#12621=CARTESIAN_POINT('Ctrl Pts',(11.4,1.45718524058191,0.));
#12622=CARTESIAN_POINT('',(11.4,1.32241589772268,0.7));
#12623=CARTESIAN_POINT('Ctrl Pts',(11.3999999999682,1.32241589773435,0.7));
#12624=CARTESIAN_POINT('Ctrl Pts',(11.4000000023735,1.33035873561384,0.69999999792071));
#12625=CARTESIAN_POINT('Ctrl Pts',(11.3999980827719,1.33823923135401,0.699006238562837));
#12626=CARTESIAN_POINT('Ctrl Pts',(11.3999964146773,1.34591623266897,0.697118452648154));
#12627=CARTESIAN_POINT('Ctrl Pts',(11.3999954805754,1.35021521026861,0.696061327733467));
#12628=CARTESIAN_POINT('Ctrl Pts',(11.3999946303028,1.35445042327231,0.694722827332644));
#12629=CARTESIAN_POINT('Ctrl Pts',(11.3999940855437,1.35859537550353,0.6931136259882));
#12630=CARTESIAN_POINT('Ctrl Pts',(11.3999931076272,1.36603612757745,0.690224891070856));
#12631=CARTESIAN_POINT('Ctrl Pts',(11.3999932937992,1.3731074395729,0.686497549823264));
#12632=CARTESIAN_POINT('Ctrl Pts',(11.3999945206258,1.37966241828116,0.682010734965951));
#12633=CARTESIAN_POINT('Ctrl Pts',(11.3999951957832,1.38326980879772,0.679541513617388));
#12634=CARTESIAN_POINT('Ctrl Pts',(11.399996159718,1.38672054258633,0.67684140394947));
#12635=CARTESIAN_POINT('Ctrl Pts',(11.3999970106794,1.38998612808193,0.67391813047908));
#12636=CARTESIAN_POINT('Ctrl Pts',(11.399997834674,1.39314822810011,0.671087494715186));
#12637=CARTESIAN_POINT('Ctrl Pts',(11.3999985616145,1.39611771109305,0.668064564866167));
#12638=CARTESIAN_POINT('Ctrl Pts',(11.3999985600482,1.39887227052748,0.664860274403491));
#12639=CARTESIAN_POINT('Ctrl Pts',(11.3999985571253,1.40401282028653,0.65888043807832));
#12640=CARTESIAN_POINT('Ctrl Pts',(11.3999962993541,1.40840780441339,0.652270325570232));
#12641=CARTESIAN_POINT('Ctrl Pts',(11.399995545677,1.411994629421,0.6451936465425));
#12642=CARTESIAN_POINT('Ctrl Pts',(11.3999954685939,1.41236147527551,0.644469872631166));
#12643=CARTESIAN_POINT('Ctrl Pts',(11.3999954033687,1.41271982702329,0.643741199273148));
#12644=CARTESIAN_POINT('Ctrl Pts',(11.399995351278,1.41306958904162,0.643007791034547));
#12645=CARTESIAN_POINT('Ctrl Pts',(11.3999948427782,1.41648390439843,0.635848388696429));
#12646=CARTESIAN_POINT('Ctrl Pts',(11.3999960181446,1.41904356023948,0.628323447569199));
#12647=CARTESIAN_POINT('Ctrl Pts',(11.3999977140636,1.42069349507095,0.620600117586001));
#12648=CARTESIAN_POINT('Ctrl Pts',(11.3999987928026,1.4217429844709,0.615687467222433));
#12649=CARTESIAN_POINT('Ctrl Pts',(11.4,1.42242354791745,0.610693903223035));
#12650=CARTESIAN_POINT('Ctrl Pts',(11.4,1.42271022042989,0.605660349289938));
#12651=CARTESIAN_POINT('',(11.4,-1.32241589772233,0.7));
#12652=CARTESIAN_POINT('',(11.4,-0.768899768518519,0.7));
#12653=CARTESIAN_POINT('Ctrl Pts',(11.4,-1.4227102204299,0.605660349289938));
#12654=CARTESIAN_POINT('Ctrl Pts',(11.4,-1.42225988230954,0.613567634148305));
#12655=CARTESIAN_POINT('Ctrl Pts',(11.399997277834,-1.42084002197897,0.621378952482038));
#12656=CARTESIAN_POINT('Ctrl Pts',(11.3999960666067,-1.41853584574224,0.62893480307212));
#12657=CARTESIAN_POINT('Ctrl Pts',(11.3999954054252,-1.41727804822547,0.633059370437125));
#12658=CARTESIAN_POINT('Ctrl Pts',(11.399995101512,-1.41575577202439,0.637107840337094));
#12659=CARTESIAN_POINT('Ctrl Pts',(11.3999952458732,-1.4139766528271,0.641052464558972));
#12660=CARTESIAN_POINT('Ctrl Pts',(11.3999955106959,-1.41071295596475,0.648288661951321));
#12661=CARTESIAN_POINT('Ctrl Pts',(11.3999975070228,-1.40662392062869,0.655096264526915));
#12662=CARTESIAN_POINT('Ctrl Pts',(11.3999983091255,-1.40177626405188,0.661313589686923));
#12663=CARTESIAN_POINT('Ctrl Pts',(11.3999984645713,-1.40083679843637,0.66251849418371));
#12664=CARTESIAN_POINT('Ctrl Pts',(11.3999985618942,-1.3998687022723,0.663701157110503));
#12665=CARTESIAN_POINT('Ctrl Pts',(11.3999985615247,-1.39887227038638,0.664860274403572));
#12666=CARTESIAN_POINT('Ctrl Pts',(11.3999985608543,-1.39706426040285,0.666963474499402));
#12667=CARTESIAN_POINT('Ctrl Pts',(11.3999982409398,-1.39516298427334,0.668989190735049));
#12668=CARTESIAN_POINT('Ctrl Pts',(11.3999977953094,-1.39317470503404,0.670934323115149));
#12669=CARTESIAN_POINT('Ctrl Pts',(11.3999965209597,-1.38748891009577,0.67649673287249));
#12670=CARTESIAN_POINT('Ctrl Pts',(11.3999944455422,-1.38115857071774,0.681340422576046));
#12671=CARTESIAN_POINT('Ctrl Pts',(11.3999937508435,-1.37434881732181,0.685413525744465));
#12672=CARTESIAN_POINT('Ctrl Pts',(11.3999933041982,-1.36997059693002,0.688032261301096));
#12673=CARTESIAN_POINT('Ctrl Pts',(11.3999933336943,-1.3653932120823,0.69033179581025));
#12674=CARTESIAN_POINT('Ctrl Pts',(11.399993839827,-1.36065445462682,0.69228884175444));
#12675=CARTESIAN_POINT('Ctrl Pts',(11.3999946245508,-1.35330733883187,0.695323106179894));
#12676=CARTESIAN_POINT('Ctrl Pts',(11.3999965692242,-1.34565642326237,0.69750197024776));
#12677=CARTESIAN_POINT('Ctrl Pts',(11.3999981510416,-1.33784990929195,0.698756936804364));
#12678=CARTESIAN_POINT('Ctrl Pts',(11.399999182603,-1.33275899381189,0.699575346749464));
#12679=CARTESIAN_POINT('Ctrl Pts',(11.4000000015384,-1.32760128986121,0.699999998642559));
#12680=CARTESIAN_POINT('Ctrl Pts',(11.3999999999682,-1.32241589773435,0.7));
#12681=CARTESIAN_POINT('Ctrl Pts',(11.227882892666,-1.47337141465794,-0.000640335460849732));
#12682=CARTESIAN_POINT('Ctrl Pts',(11.218588765022,-1.46278323638644,0.201451598614313));
#12683=CARTESIAN_POINT('Ctrl Pts',(11.2092944683555,-1.45219508216535,0.40354352620373));
#12684=CARTESIAN_POINT('Ctrl Pts',(11.2000000000001,-1.44160695250309,0.60563544721184));
#12685=CARTESIAN_POINT('Ctrl Pts',(10.1843397214697,-1.57034855377304,-0.000384310983874139));
#12686=CARTESIAN_POINT('Ctrl Pts',(10.1768953195658,-1.55975965902304,0.201708049868595));
#12687=CARTESIAN_POINT('Ctrl Pts',(10.1694507716805,-1.54917076711515,0.403800406245857));
#12688=CARTESIAN_POINT('Ctrl Pts',(10.1620060668616,-1.53858190981164,0.605892758286982));
#12689=CARTESIAN_POINT('Ctrl Pts',(9.14170648965309,-1.65016851777514,-0.000148134864058495));
#12690=CARTESIAN_POINT('Ctrl Pts',(9.13611341817177,-1.63957870617509,0.201944615677573));
#12691=CARTESIAN_POINT('Ctrl Pts',(9.13052023035058,-1.6289888900612,0.404037363603497));
#12692=CARTESIAN_POINT('Ctrl Pts',(9.124926910836,-1.6183991014662,0.606130109186173));
#12693=CARTESIAN_POINT('Ctrl Pts',(8.1,-1.69866351109718,1.00613961606655E-16));
#12694=CARTESIAN_POINT('Ctrl Pts',(8.09625995443094,-1.68807302815665,0.202092993803311));
#12695=CARTESIAN_POINT('Ctrl Pts',(8.09251982249141,-1.67748255132318,0.404185986335255));
#12696=CARTESIAN_POINT('Ctrl Pts',(8.08877960280056,-1.66689208072706,0.606278977577217));
#12697=CARTESIAN_POINT('Ctrl Pts',(8.1,-1.66641703131627,0.605314487869832));
#12698=CARTESIAN_POINT('Ctrl Pts',(9.13548525483003,-1.617718421277,0.605389190939432));
#12699=CARTESIAN_POINT('Ctrl Pts',(10.168822041161,-1.53796707615457,0.605507632815633));
#12700=CARTESIAN_POINT('Ctrl Pts',(11.2000000000893,-1.44160695345912,0.605635447210802));
#12701=CARTESIAN_POINT('Ctrl Pts',(11.7095939787209,-1.42740645209206,-7.69249563980189E-5));
#12702=CARTESIAN_POINT('Ctrl Pts',(11.6994545874061,-1.41682738380082,0.201847033339061));
#12703=CARTESIAN_POINT('Ctrl Pts',(11.6893150192885,-1.40624834198077,0.403770984173611));
#12704=CARTESIAN_POINT('Ctrl Pts',(11.6791752715866,-1.39566932719028,0.605694927437301));
#12705=CARTESIAN_POINT('Ctrl Pts',(11.6063871276792,-1.43748358609578,-5.11721697277706E-5));
#12706=CARTESIAN_POINT('Ctrl Pts',(11.596430427176,-1.42690445239132,0.201872829148883));
#12707=CARTESIAN_POINT('Ctrl Pts',(11.5864735514701,-1.41632534465399,0.403796823219986));
#12708=CARTESIAN_POINT('Ctrl Pts',(11.5765164978042,-1.40574626343445,0.605720809936841));
#12709=CARTESIAN_POINT('Ctrl Pts',(11.5031891278894,-1.4474144288224,-2.55082377288765E-5));
#12710=CARTESIAN_POINT('Ctrl Pts',(11.4934151336386,-1.43683522760458,0.201898535909597));
#12711=CARTESIAN_POINT('Ctrl Pts',(11.4836409658656,-1.42625605183456,0.40382257302165));
#12712=CARTESIAN_POINT('Ctrl Pts',(11.4738666218385,-1.41567690205216,0.605746602994839));
#12713=CARTESIAN_POINT('Ctrl Pts',(11.4,-1.45718524058191,-5.20417042793042E-18));
#12714=CARTESIAN_POINT('Ctrl Pts',(11.3904087275488,-1.44660597001679,0.201924086674796));
#12715=CARTESIAN_POINT('Ctrl Pts',(11.3808172833376,-1.43602672436683,0.403848166524883));
#12716=CARTESIAN_POINT('Ctrl Pts',(11.3712256646606,-1.42544750415802,0.605772239449758));
#12717=CARTESIAN_POINT('',(11.6778970386953,-1.39579479040469,0.605695249702977));
#12718=CARTESIAN_POINT('Ctrl Pts',(11.4,-1.4227102204299,0.605660349289938));
#12719=CARTESIAN_POINT('Ctrl Pts',(11.4926474653491,-1.41386220753305,0.605671932550561));
#12720=CARTESIAN_POINT('Ctrl Pts',(11.585279512325,-1.40488700096013,0.605683574233495));
#12721=CARTESIAN_POINT('Ctrl Pts',(11.6778970386953,-1.39579479040469,0.605695249702977));
#12722=CARTESIAN_POINT('Ctrl Pts',(11.6778970386953,-1.39579479040469,0.605695249702977));
#12723=CARTESIAN_POINT('Ctrl Pts',(11.6884613130147,-1.40633044792991,0.403796817797553));
#12724=CARTESIAN_POINT('Ctrl Pts',(11.6990256725537,-1.41686632615463,0.201898401304098));
#12725=CARTESIAN_POINT('Ctrl Pts',(11.7095901160181,-1.42740242188993,5.19332840620557E-17));
#12726=CARTESIAN_POINT('Ctrl Pts',(11.2,-1.34133050917871,0.7));
#12727=CARTESIAN_POINT('Ctrl Pts',(10.1668086441106,-1.43797263608903,0.7));
#12728=CARTESIAN_POINT('Ctrl Pts',(9.13190264019122,-1.51792184128158,0.7));
#12729=CARTESIAN_POINT('Ctrl Pts',(8.09530923905977,-1.56666858280461,0.7));
#12730=CARTESIAN_POINT('Ctrl Pts',(11.2026864299662,-1.37005086445236,0.7));
#12731=CARTESIAN_POINT('Ctrl Pts',(10.1691860218014,-1.46674693471719,0.700000910790016));
#12732=CARTESIAN_POINT('Ctrl Pts',(9.13384227773975,-1.54675516497,0.699999464833944));
#12733=CARTESIAN_POINT('Ctrl Pts',(8.09666712422266,-1.59554384206015,0.700000000000001));
#12734=CARTESIAN_POINT('Ctrl Pts',(11.2073428085028,-1.4198317437391,0.676744232988519));
#12735=CARTESIAN_POINT('Ctrl Pts',(10.1733099382853,-1.51661799675652,0.676702307311825));
#12736=CARTESIAN_POINT('Ctrl Pts',(9.13719745543551,-1.59672983278297,0.676663906627884));
#12737=CARTESIAN_POINT('Ctrl Pts',(8.09902054834098,-1.64558911349573,0.676639354455264));
#12738=CARTESIAN_POINT('Ctrl Pts',(11.2091847227485,-1.43952346553595,0.627236497176141));
#12739=CARTESIAN_POINT('Ctrl Pts',(10.1749352046592,-1.53629892039422,0.62712791425818));
#12740=CARTESIAN_POINT('Ctrl Pts',(9.13852107143019,-1.61640633519008,0.627027713743691));
#12741=CARTESIAN_POINT('Ctrl Pts',(8.0999458765183,-1.66526610220338,0.626964226563296));
#12742=CARTESIAN_POINT('Ctrl Pts',(11.209298290232,-1.4407376041935,0.605636599993194));
#12743=CARTESIAN_POINT('Ctrl Pts',(10.1750338985877,-1.53748737250229,0.605508345221004));
#12744=CARTESIAN_POINT('Ctrl Pts',(9.13859765097935,-1.61757204607208,0.605389415477198));
#12745=CARTESIAN_POINT('Ctrl Pts',(8.1,-1.66641703131627,0.605314487869832));
#12746=CARTESIAN_POINT('Ctrl Pts',(11.2,-1.34133050917871,0.7));
#12747=CARTESIAN_POINT('Ctrl Pts',(10.16836710286,-1.43782686176815,0.7));
#12748=CARTESIAN_POINT('Ctrl Pts',(9.13502472651537,-1.51768061363633,0.7));
#12749=CARTESIAN_POINT('Ctrl Pts',(8.09999999865516,-1.56644778212326,0.7));
#12750=CARTESIAN_POINT('Ctrl Pts',(11.6681436286308,-1.2964346619681,0.7));
#12751=CARTESIAN_POINT('Ctrl Pts',(11.5756099286391,-1.3055179747114,0.7));
#12752=CARTESIAN_POINT('Ctrl Pts',(11.4830653488871,-1.31448403714215,0.7));
#12753=CARTESIAN_POINT('Ctrl Pts',(11.3905090053564,-1.32332268868375,0.7));
#12754=CARTESIAN_POINT('Ctrl Pts',(11.6709605510772,-1.32513126902304,0.700000000000001));
#12755=CARTESIAN_POINT('Ctrl Pts',(11.5784027531871,-1.33421922733773,0.700000082825348));
#12756=CARTESIAN_POINT('Ctrl Pts',(11.4858332859074,-1.34318985044544,0.699999917777441));
#12757=CARTESIAN_POINT('Ctrl Pts',(11.3932507170007,-1.35203326785046,0.7));
#12758=CARTESIAN_POINT('Ctrl Pts',(11.6758431636759,-1.37487151491717,0.67676311428296));
#12759=CARTESIAN_POINT('Ctrl Pts',(11.583243842395,-1.38396722707511,0.676759299309384));
#12760=CARTESIAN_POINT('Ctrl Pts',(11.4906306781253,-1.39294591144353,0.676755553516685));
#12761=CARTESIAN_POINT('Ctrl Pts',(11.3980029235659,-1.40179729139028,0.67675176769038));
#12762=CARTESIAN_POINT('Ctrl Pts',(11.6777767156198,-1.39456903283364,0.627286048421068));
#12763=CARTESIAN_POINT('Ctrl Pts',(11.5851604051362,-1.40366358810601,0.627276165220861));
#12764=CARTESIAN_POINT('Ctrl Pts',(11.4925297866457,-1.41264104586547,0.627266369072496));
#12765=CARTESIAN_POINT('Ctrl Pts',(11.3998836071583,-1.4214913811319,0.627256563056779));
#12766=CARTESIAN_POINT('Ctrl Pts',(11.6778970386953,-1.39579479040469,0.605695249702977));
#12767=CARTESIAN_POINT('Ctrl Pts',(11.585279512325,-1.40488700096013,0.605683574233495));
#12768=CARTESIAN_POINT('Ctrl Pts',(11.4926474653491,-1.41386220753305,0.605671932550561));
#12769=CARTESIAN_POINT('Ctrl Pts',(11.4,-1.4227102204299,0.605660349289938));
#12770=CARTESIAN_POINT('',(11.6681436286308,-1.2964346619681,0.7));
#12771=CARTESIAN_POINT('Ctrl Pts',(11.6681436286308,-1.2964346619681,0.7));
#12772=CARTESIAN_POINT('Ctrl Pts',(11.5787728332608,-1.30520749699507,0.7));
#12773=CARTESIAN_POINT('Ctrl Pts',(11.4893918891838,-1.31387096021207,0.7));
#12774=CARTESIAN_POINT('Ctrl Pts',(11.3999999999682,-1.32241589773435,0.7));
#12775=CARTESIAN_POINT('Origin',(11.6681436286308,-1.2964346619681,0.6));
#12776=CARTESIAN_POINT('Origin',(6.08012166120517,1.06778195214465E-16,
0.7));
#12777=CARTESIAN_POINT('Ctrl Pts',(8.0999999986552,1.56644778212326,0.7));
#12778=CARTESIAN_POINT('Ctrl Pts',(9.13502472651542,1.51768061363633,0.7));
#12779=CARTESIAN_POINT('Ctrl Pts',(10.16836710286,1.43782686176815,0.7));
#12780=CARTESIAN_POINT('Ctrl Pts',(11.2,1.34133050917871,0.7));
#12781=CARTESIAN_POINT('Origin',(6.08012166120517,1.06778195214465E-16,
0.7));
#12782=CARTESIAN_POINT('',(11.6681436286308,1.2964346619681,0.7));
#12783=CARTESIAN_POINT('Ctrl Pts',(11.3999999999682,1.32241589773435,0.7));
#12784=CARTESIAN_POINT('Ctrl Pts',(11.4893918891837,1.31387096021208,0.7));
#12785=CARTESIAN_POINT('Ctrl Pts',(11.5787728332608,1.30520749699508,0.7));
#12786=CARTESIAN_POINT('Ctrl Pts',(11.6681436286308,1.2964346619681,0.7));
#12787=CARTESIAN_POINT('',(11.6681436286308,0.8,0.7));
#12788=CARTESIAN_POINT('Ctrl Pts',(8.09530923905978,1.56666858280461,0.7));
#12789=CARTESIAN_POINT('Ctrl Pts',(9.13190264019124,1.51792184128158,0.7));
#12790=CARTESIAN_POINT('Ctrl Pts',(10.1668086441106,1.43797263608903,0.7));
#12791=CARTESIAN_POINT('Ctrl Pts',(11.2,1.34133050917871,0.7));
#12792=CARTESIAN_POINT('Ctrl Pts',(8.09666712422266,1.59554384206015,0.700000000000001));
#12793=CARTESIAN_POINT('Ctrl Pts',(9.13384227773977,1.54675516497,0.699999464833944));
#12794=CARTESIAN_POINT('Ctrl Pts',(10.1691860218013,1.46674693471719,0.700000910790016));
#12795=CARTESIAN_POINT('Ctrl Pts',(11.2026864299662,1.37005086445236,0.7));
#12796=CARTESIAN_POINT('Ctrl Pts',(8.09902054834099,1.64558911349573,0.676639354455264));
#12797=CARTESIAN_POINT('Ctrl Pts',(9.13719745543553,1.59672983278297,0.676663906627884));
#12798=CARTESIAN_POINT('Ctrl Pts',(10.1733099382853,1.51661799675652,0.676702307311825));
#12799=CARTESIAN_POINT('Ctrl Pts',(11.2073428085028,1.4198317437391,0.676744232988519));
#12800=CARTESIAN_POINT('Ctrl Pts',(8.0999458765183,1.66526610220338,0.626964226563296));
#12801=CARTESIAN_POINT('Ctrl Pts',(9.1385210714302,1.61640633519008,0.627027713743691));
#12802=CARTESIAN_POINT('Ctrl Pts',(10.1749352046592,1.53629892039423,0.62712791425818));
#12803=CARTESIAN_POINT('Ctrl Pts',(11.2091847227485,1.43952346553595,0.627236497176141));
#12804=CARTESIAN_POINT('Ctrl Pts',(8.1,1.66641703131627,0.605314487869832));
#12805=CARTESIAN_POINT('Ctrl Pts',(9.13859765097937,1.61757204607208,0.605389415477198));
#12806=CARTESIAN_POINT('Ctrl Pts',(10.1750338985877,1.53748737250229,0.605508345221004));
#12807=CARTESIAN_POINT('Ctrl Pts',(11.209298290232,1.4407376041935,0.605636599993194));
#12808=CARTESIAN_POINT('Ctrl Pts',(11.2000000000893,1.44160695345912,0.605635447210802));
#12809=CARTESIAN_POINT('Ctrl Pts',(10.168822041161,1.53796707615457,0.605507632815633));
#12810=CARTESIAN_POINT('Ctrl Pts',(9.13548525483005,1.617718421277,0.605389190939432));
#12811=CARTESIAN_POINT('Ctrl Pts',(8.1,1.66641703131627,0.605314487869832));
#12812=CARTESIAN_POINT('Ctrl Pts',(8.1,1.69866351109859,-2.6441702993818E-11));
#12813=CARTESIAN_POINT('Ctrl Pts',(8.09625995443078,1.68807302815759,0.202092993785684));
#12814=CARTESIAN_POINT('Ctrl Pts',(8.09251982249108,1.67748255132366,0.404185986326441));
#12815=CARTESIAN_POINT('Ctrl Pts',(8.08877960280008,1.66689208072708,0.606278977577217));
#12816=CARTESIAN_POINT('Ctrl Pts',(9.14170648965349,1.65016851777655,-0.00014813489050026));
#12817=CARTESIAN_POINT('Ctrl Pts',(9.13611341817193,1.63957870617604,0.201944615659945));
#12818=CARTESIAN_POINT('Ctrl Pts',(9.1305202303505,1.62898889006169,0.404037363594684));
#12819=CARTESIAN_POINT('Ctrl Pts',(9.12492691083567,1.61839910146622,0.606130109186173));
#12820=CARTESIAN_POINT('Ctrl Pts',(10.1843397214705,1.57034855377444,-0.000384311010315772));
#12821=CARTESIAN_POINT('Ctrl Pts',(10.1768953195662,1.55975965902398,0.201708049850968));
#12822=CARTESIAN_POINT('Ctrl Pts',(10.1694507716807,1.54917076711562,0.403800406237042));
#12823=CARTESIAN_POINT('Ctrl Pts',(10.1620060668615,1.53858190981166,0.605892758286982));
#12824=CARTESIAN_POINT('Ctrl Pts',(11.2278828926672,1.47337141465933,-0.000640335487291374));
#12825=CARTESIAN_POINT('Ctrl Pts',(11.2185887650228,1.46278323638736,0.201451598596686));
#12826=CARTESIAN_POINT('Ctrl Pts',(11.2092944683559,1.45219508216582,0.403543526194916));
#12827=CARTESIAN_POINT('Ctrl Pts',(11.2000000000001,1.44160695250309,0.60563544721184));
#12828=CARTESIAN_POINT('Ctrl Pts',(11.4,1.45718524058191,-1.37043154602168E-16));
#12829=CARTESIAN_POINT('Ctrl Pts',(11.3904087275488,1.44660597001679,0.201924086674796));
#12830=CARTESIAN_POINT('Ctrl Pts',(11.3808172833376,1.43602672436683,0.403848166524884));
#12831=CARTESIAN_POINT('Ctrl Pts',(11.3712256646606,1.42544750415802,0.605772239449759));
#12832=CARTESIAN_POINT('Ctrl Pts',(11.5031891278894,1.4474144288224,-2.55082377290153E-5));
#12833=CARTESIAN_POINT('Ctrl Pts',(11.4934151336386,1.43683522760458,0.201898535909598));
#12834=CARTESIAN_POINT('Ctrl Pts',(11.4836409658656,1.42625605183455,0.40382257302165));
#12835=CARTESIAN_POINT('Ctrl Pts',(11.4738666218385,1.41567690205216,0.605746602994839));
#12836=CARTESIAN_POINT('Ctrl Pts',(11.6063871276792,1.43748358609579,-5.1172169727805E-5));
#12837=CARTESIAN_POINT('Ctrl Pts',(11.596430427176,1.42690445239132,0.201872829148883));
#12838=CARTESIAN_POINT('Ctrl Pts',(11.5864735514701,1.41632534465399,0.403796823219986));
#12839=CARTESIAN_POINT('Ctrl Pts',(11.5765164978042,1.40574626343445,0.605720809936842));
#12840=CARTESIAN_POINT('Ctrl Pts',(11.7095939787209,1.42740645209206,-7.69249563980588E-5));
#12841=CARTESIAN_POINT('Ctrl Pts',(11.6994545874061,1.41682738380082,0.201847033339061));
#12842=CARTESIAN_POINT('Ctrl Pts',(11.6893150192885,1.40624834198077,0.403770984173611));
#12843=CARTESIAN_POINT('Ctrl Pts',(11.6791752715866,1.39566932719028,0.605694927437301));
#12844=CARTESIAN_POINT('',(11.6778970386953,1.39579479040469,0.605695249702977));
#12845=CARTESIAN_POINT('Ctrl Pts',(11.7095901160181,1.42740242188993,2.01986864734049E-16));
#12846=CARTESIAN_POINT('Ctrl Pts',(11.6990256725537,1.41686632615463,0.201898401304098));
#12847=CARTESIAN_POINT('Ctrl Pts',(11.6884613130147,1.40633044792991,0.403796817797553));
#12848=CARTESIAN_POINT('Ctrl Pts',(11.6778970386953,1.39579479040469,0.605695249702978));
#12849=CARTESIAN_POINT('Ctrl Pts',(11.6778970386953,1.39579479040469,0.605695249702977));
#12850=CARTESIAN_POINT('Ctrl Pts',(11.585279512325,1.40488700096013,0.605683574233495));
#12851=CARTESIAN_POINT('Ctrl Pts',(11.4926474653491,1.41386220753305,0.605671932550561));
#12852=CARTESIAN_POINT('Ctrl Pts',(11.4,1.4227102204299,0.605660349289938));
#12853=CARTESIAN_POINT('Origin',(7.9,1.7737037037037,0.));
#12854=CARTESIAN_POINT('',(7.9,-1.67543132363858,0.605300614462415));
#12855=CARTESIAN_POINT('Ctrl Pts',(7.9,-1.67543132363858,0.605300614462415));
#12856=CARTESIAN_POINT('Ctrl Pts',(7.9,-1.68078196203297,0.504592238472094));
#12857=CARTESIAN_POINT('Ctrl Pts',(7.9,-1.68613236521525,0.403883028813119));
#12858=CARTESIAN_POINT('Ctrl Pts',(7.9,-1.69685110017509,0.202116711316755));
#12859=CARTESIAN_POINT('Ctrl Pts',(7.9,-1.70221951791351,0.10105794916591));
#12860=CARTESIAN_POINT('Ctrl Pts',(7.9,-1.70758761671949,0.));
#12861=CARTESIAN_POINT('',(7.9,-1.57547905376932,0.7));
#12862=CARTESIAN_POINT('Ctrl Pts',(7.9,-1.57547905376882,0.7));
#12863=CARTESIAN_POINT('Ctrl Pts',(7.9,-1.58339333479856,0.700000000000001));
#12864=CARTESIAN_POINT('Ctrl Pts',(7.89999913038498,-1.59124411312484,0.699006032637452));
#12865=CARTESIAN_POINT('Ctrl Pts',(7.89999837104309,-1.59889106951376,0.697118831203047));
#12866=CARTESIAN_POINT('Ctrl Pts',(7.89999794343345,-1.6031973145812,0.696056087876834));
#12867=CARTESIAN_POINT('Ctrl Pts',(7.89999755365678,-1.60743898057435,0.694709047589066));
#12868=CARTESIAN_POINT('Ctrl Pts',(7.89999730661842,-1.61158931211603,0.693088720937666));
#12869=CARTESIAN_POINT('Ctrl Pts',(7.89999686465941,-1.6190143793929,0.690189908089508));
#12870=CARTESIAN_POINT('Ctrl Pts',(7.89999696143539,-1.626066934352,0.686450944759811));
#12871=CARTESIAN_POINT('Ctrl Pts',(7.89999752554231,-1.63260082031789,0.681953255064161));
#12872=CARTESIAN_POINT('Ctrl Pts',(7.89999783650325,-1.63620259020663,0.679473927540052));
#12873=CARTESIAN_POINT('Ctrl Pts',(7.89999827825103,-1.63964648551863,0.676763160200805));
#12874=CARTESIAN_POINT('Ctrl Pts',(7.89999867021687,-1.64290407802379,0.673829034208746));
#12875=CARTESIAN_POINT('Ctrl Pts',(7.89999905115172,-1.64606999298761,0.670977482527793));
#12876=CARTESIAN_POINT('Ctrl Pts',(7.89999938859403,-1.64904076201529,0.667932171841817));
#12877=CARTESIAN_POINT('Ctrl Pts',(7.89999938783828,-1.6517939440564,0.66470449824639));
#12878=CARTESIAN_POINT('Ctrl Pts',(7.89999938643498,-1.65690611124346,0.658711285012161));
#12879=CARTESIAN_POINT('Ctrl Pts',(7.89999834643869,-1.661271022418,0.652090721578155));
#12880=CARTESIAN_POINT('Ctrl Pts',(7.89999799057748,-1.66482884904143,0.645008203309728));
#12881=CARTESIAN_POINT('Ctrl Pts',(7.89999795399159,-1.66519462718329,0.644280053614395));
#12882=CARTESIAN_POINT('Ctrl Pts',(7.89999792287445,-1.66555183396469,0.643547001244109));
#12883=CARTESIAN_POINT('Ctrl Pts',(7.89999789784292,-1.66590037542058,0.642809214685104));
#12884=CARTESIAN_POINT('Ctrl Pts',(7.89999765441981,-1.66928982250308,0.635634491398386));
#12885=CARTESIAN_POINT('Ctrl Pts',(7.89999817709027,-1.67182454272713,0.628096763436417));
#12886=CARTESIAN_POINT('Ctrl Pts',(7.8999989464625,-1.67345106343068,0.620364350320046));
#12887=CARTESIAN_POINT('Ctrl Pts',(7.89999943944948,-1.67449328136075,0.615409688768565));
#12888=CARTESIAN_POINT('Ctrl Pts',(7.89999999630063,-1.67516175160204,0.610374426093907));
#12889=CARTESIAN_POINT('Ctrl Pts',(7.89999999769359,-1.67543132314592,0.605300614465834));
#12890=CARTESIAN_POINT('',(7.9,1.57547905376882,0.7));
#12891=CARTESIAN_POINT('',(7.9,0.886851851851852,0.7));
#12892=CARTESIAN_POINT('',(7.9,1.67543132363858,0.605300614462415));
#12893=CARTESIAN_POINT('Ctrl Pts',(7.89999999769359,1.67543132314592,0.605300614465834));
#12894=CARTESIAN_POINT('Ctrl Pts',(7.89999999552123,1.67501091691767,0.613213400729193));
#12895=CARTESIAN_POINT('Ctrl Pts',(7.89999875799714,1.67362284400845,0.621034919585595));
#12896=CARTESIAN_POINT('Ctrl Pts',(7.89999821041927,1.67135120200026,0.628604813990272));
#12897=CARTESIAN_POINT('Ctrl Pts',(7.89999790518813,1.67008494211401,0.632824428521627));
#12898=CARTESIAN_POINT('Ctrl Pts',(7.89999777089825,1.66854314417455,0.636965893954691));
#12899=CARTESIAN_POINT('Ctrl Pts',(7.89999784944871,1.66673368022774,0.640999456224326));
#12900=CARTESIAN_POINT('Ctrl Pts',(7.89999799035603,1.66348778281681,0.648235040746992));
#12901=CARTESIAN_POINT('Ctrl Pts',(7.8999989183875,1.65941887886545,0.655045206964536));
#12902=CARTESIAN_POINT('Ctrl Pts',(7.89999927807636,1.65459101651367,0.661266862646797));
#12903=CARTESIAN_POINT('Ctrl Pts',(7.89999934554656,1.65368540929837,0.662433916689859));
#12904=CARTESIAN_POINT('Ctrl Pts',(7.89999938740919,1.65275296801062,0.663580193269421));
#12905=CARTESIAN_POINT('Ctrl Pts',(7.89999938728957,1.65179394408007,0.664704498246374));
#12906=CARTESIAN_POINT('Ctrl Pts',(7.89999938705343,1.64990069294102,0.666924037937161));
#12907=CARTESIAN_POINT('Ctrl Pts',(7.89999922461202,1.64790387543569,0.669057997255949));
#12908=CARTESIAN_POINT('Ctrl Pts',(7.89999900301747,1.64581073954063,0.671102663899023));
#12909=CARTESIAN_POINT('Ctrl Pts',(7.89999840121276,1.64012621790684,0.676655553128015));
#12910=CARTESIAN_POINT('Ctrl Pts',(7.89999746538644,1.63379824275617,0.681490110487894));
#12911=CARTESIAN_POINT('Ctrl Pts',(7.89999715581736,1.6269906793715,0.685552192443336));
#12912=CARTESIAN_POINT('Ctrl Pts',(7.89999695885968,1.62265949106942,0.688136618155352));
#12913=CARTESIAN_POINT('Ctrl Pts',(7.89999697413705,1.61813320929371,0.690407672840119));
#12914=CARTESIAN_POINT('Ctrl Pts',(7.89999720528031,1.61344832872307,0.692342105328139));
#12915=CARTESIAN_POINT('Ctrl Pts',(7.89999756646959,1.60612763680413,0.69536488980882));
#12916=CARTESIAN_POINT('Ctrl Pts',(7.89999845750109,1.59850458633822,0.69753330980446));
#12917=CARTESIAN_POINT('Ctrl Pts',(7.89999917312139,1.59072625322659,0.698777780766876));
#12918=CARTESIAN_POINT('Ctrl Pts',(7.8999996358458,1.58569673594883,0.699582463224842));
#12919=CARTESIAN_POINT('Ctrl Pts',(7.9,1.58060170040825,0.7));
#12920=CARTESIAN_POINT('Ctrl Pts',(7.9,1.57547905376882,0.7));
#12921=CARTESIAN_POINT('Ctrl Pts',(7.9,1.70758761671949,0.));
#12922=CARTESIAN_POINT('Ctrl Pts',(7.9,1.70221949782947,0.101058327261027));
#12923=CARTESIAN_POINT('Ctrl Pts',(7.9,1.69685105999395,0.202117467714));
#12924=CARTESIAN_POINT('Ctrl Pts',(7.9,1.68613232500772,0.403883785628764));
#12925=CARTESIAN_POINT('Ctrl Pts',(7.9,1.6807819419292,0.504592616860323));
#12926=CARTESIAN_POINT('Ctrl Pts',(7.9,1.67543132363858,0.605300614462415));
#12927=CARTESIAN_POINT('Ctrl Pts',(7.91019312999368,-1.70715886092982,-0.000134090250286965));
#12928=CARTESIAN_POINT('Ctrl Pts',(7.90679525219671,-1.69658223918655,0.201692187253877));
#12929=CARTESIAN_POINT('Ctrl Pts',(7.90339729501941,-1.68600562260833,0.40351846369823));
#12930=CARTESIAN_POINT('Ctrl Pts',(7.89999925719352,-1.67542901130525,0.605344739067286));
#12931=CARTESIAN_POINT('Ctrl Pts',(6.63535348802246,-1.76179300886274,3.38453142643293E-5));
#12932=CARTESIAN_POINT('Ctrl Pts',(6.63422081661327,-1.7512156246026,0.201860399405878));
#12933=CARTESIAN_POINT('Ctrl Pts',(6.6330881724013,-1.74063821514668,0.403686949685767));
#12934=CARTESIAN_POINT('Ctrl Pts',(6.63195543348167,-1.7300608292057,0.605513504373875));
#12935=CARTESIAN_POINT('Ctrl Pts',(5.36191629096386,-1.76821426310706,6.25694230841134E-5));
#12936=CARTESIAN_POINT('Ctrl Pts',(5.36305144950513,-1.75763653444312,0.201889164820622));
#12937=CARTESIAN_POINT('Ctrl Pts',(5.36418670601529,-1.74705878452761,0.403715755186214));
#12938=CARTESIAN_POINT('Ctrl Pts',(5.36532191986746,-1.73648104871457,0.605542351516859));
#12939=CARTESIAN_POINT('Ctrl Pts',(4.08978435919194,-1.70060618495018,-0.000163379468877527));
#12940=CARTESIAN_POINT('Ctrl Pts',(4.09318947412453,-1.69002991101751,0.201662855819258));
#12941=CARTESIAN_POINT('Ctrl Pts',(4.09659468720556,-1.67945364498778,0.403489089874722));
#12942=CARTESIAN_POINT('Ctrl Pts',(4.1,-1.66887738702936,0.605315322680078));
#12943=CARTESIAN_POINT('Ctrl Pts',(4.10000000006189,-1.66887738587128,0.605315322687833));
#12944=CARTESIAN_POINT('Ctrl Pts',(5.36600428635239,-1.73653511802878,0.605201749988751));
#12945=CARTESIAN_POINT('Ctrl Pts',(6.63469107356441,-1.72995836404769,0.605216415547347));
#12946=CARTESIAN_POINT('Ctrl Pts',(7.89999999997453,-1.67543132304763,0.605300614465986));
#12947=CARTESIAN_POINT('Ctrl Pts',(7.9,-1.57547905376882,0.7));
#12948=CARTESIAN_POINT('Ctrl Pts',(6.63400208894818,-1.63014048526579,0.7));
#12949=CARTESIAN_POINT('Ctrl Pts',(5.36531976402288,-1.63670020240541,0.7));
#12950=CARTESIAN_POINT('Ctrl Pts',(4.09999999999999,-1.56887583540973,0.7));
#12951=CARTESIAN_POINT('Ctrl Pts',(7.9012470621039,-1.60436190544783,0.700000000000001));
#12952=CARTESIAN_POINT('Ctrl Pts',(6.6345175325877,-1.65907137725265,0.700000604190856));
#12953=CARTESIAN_POINT('Ctrl Pts',(5.36490325870521,-1.66564852467601,0.700000815814724));
#12954=CARTESIAN_POINT('Ctrl Pts',(4.09845273665223,-1.59774131518914,0.699999999999999));
#12955=CARTESIAN_POINT('Ctrl Pts',(7.90340849276168,-1.6544221878571,0.676636720659303));
#12956=CARTESIAN_POINT('Ctrl Pts',(6.63541917043928,-1.70921256696412,0.676609005714152));
#12957=CARTESIAN_POINT('Ctrl Pts',(5.36416860778507,-1.71581908642683,0.67660414986632));
#12958=CARTESIAN_POINT('Ctrl Pts',(4.09577098158984,-1.64777167791894,0.676641578059328));
#12959=CARTESIAN_POINT('Ctrl Pts',(7.90425799286387,-1.67409721877663,0.626952737571144));
#12960=CARTESIAN_POINT('Ctrl Pts',(6.63576820027036,-1.72888861107585,0.626881076846221));
#12961=CARTESIAN_POINT('Ctrl Pts',(5.36388821219926,-1.73550154452763,0.626868555890157));
#12962=CARTESIAN_POINT('Ctrl Pts',(4.09471668402893,-1.66744047248441,0.626965338598652));
#12963=CARTESIAN_POINT('Ctrl Pts',(7.90430757201307,-1.67524550738887,0.605300901379154));
#12964=CARTESIAN_POINT('Ctrl Pts',(6.63578978311492,-1.73002023206136,0.605216330280387));
#12965=CARTESIAN_POINT('Ctrl Pts',(5.3638700255334,-1.7366305488338,0.605201579557148));
#12966=CARTESIAN_POINT('Ctrl Pts',(4.09465499692593,-1.6685912965035,0.605315802949303));
#12967=CARTESIAN_POINT('Ctrl Pts',(7.9,-1.57547905376882,0.7));
#12968=CARTESIAN_POINT('Ctrl Pts',(6.63400208894818,-1.63014048526579,0.7));
#12969=CARTESIAN_POINT('Ctrl Pts',(5.36531976402288,-1.63670020240541,0.7));
#12970=CARTESIAN_POINT('Ctrl Pts',(4.09999999999999,-1.56887583540973,0.7));
#12971=CARTESIAN_POINT('Origin',(6.08012166120517,1.06778195214465E-16,
0.7));
#12972=CARTESIAN_POINT('Ctrl Pts',(4.1,1.56887583540973,0.7));
#12973=CARTESIAN_POINT('Ctrl Pts',(5.36531976402291,1.63670020240541,0.7));
#12974=CARTESIAN_POINT('Ctrl Pts',(6.63400208894819,1.63014048526579,0.7));
#12975=CARTESIAN_POINT('Ctrl Pts',(7.9,1.57547905376882,0.7));
#12976=CARTESIAN_POINT('Ctrl Pts',(4.1,1.56887583540973,0.7));
#12977=CARTESIAN_POINT('Ctrl Pts',(5.36531976402291,1.63670020240541,0.7));
#12978=CARTESIAN_POINT('Ctrl Pts',(6.63400208894819,1.63014048526579,0.7));
#12979=CARTESIAN_POINT('Ctrl Pts',(7.9,1.57547905376882,0.7));
#12980=CARTESIAN_POINT('Ctrl Pts',(4.09845273665224,1.59774131518914,0.699999999999999));
#12981=CARTESIAN_POINT('Ctrl Pts',(5.36490325870523,1.66564852467601,0.700000815814725));
#12982=CARTESIAN_POINT('Ctrl Pts',(6.6345175325877,1.65907137725265,0.700000604190856));
#12983=CARTESIAN_POINT('Ctrl Pts',(7.9012470621039,1.60436190544783,0.700000000000001));
#12984=CARTESIAN_POINT('Ctrl Pts',(4.09577098158985,1.64777167791894,0.676641578059328));
#12985=CARTESIAN_POINT('Ctrl Pts',(5.36416860778509,1.71581908642683,0.67660414986632));
#12986=CARTESIAN_POINT('Ctrl Pts',(6.6354191704393,1.70921256696412,0.676609005714152));
#12987=CARTESIAN_POINT('Ctrl Pts',(7.90340849276168,1.6544221878571,0.676636720659302));
#12988=CARTESIAN_POINT('Ctrl Pts',(4.09471668402895,1.66744047248441,0.626965338598652));
#12989=CARTESIAN_POINT('Ctrl Pts',(5.36388821219928,1.73550154452763,0.626868555890157));
#12990=CARTESIAN_POINT('Ctrl Pts',(6.63576820027036,1.72888861107585,0.626881076846221));
#12991=CARTESIAN_POINT('Ctrl Pts',(7.90425799286387,1.67409721877663,0.626952737571144));
#12992=CARTESIAN_POINT('Ctrl Pts',(4.09465499692594,1.6685912965035,0.605315802949303));
#12993=CARTESIAN_POINT('Ctrl Pts',(5.36387002553342,1.7366305488338,0.605201579557148));
#12994=CARTESIAN_POINT('Ctrl Pts',(6.63578978311492,1.73002023206136,0.605216330280387));
#12995=CARTESIAN_POINT('Ctrl Pts',(7.90430757201307,1.67524550738887,0.605300901379154));
#12996=CARTESIAN_POINT('Ctrl Pts',(7.89999999997454,1.67543132304763,0.605300614465986));
#12997=CARTESIAN_POINT('Ctrl Pts',(6.63469107356441,1.72995836404769,0.605216415547348));
#12998=CARTESIAN_POINT('Ctrl Pts',(5.36600428635241,1.73653511802878,0.605201749988751));
#12999=CARTESIAN_POINT('Ctrl Pts',(4.10000000006189,1.66887738587128,0.605315322687833));
#13000=CARTESIAN_POINT('Ctrl Pts',(4.08978435969213,1.70060618339657,-0.000163349821525811));
#13001=CARTESIAN_POINT('Ctrl Pts',(4.093189474458,1.69002990998177,0.201662875584159));
#13002=CARTESIAN_POINT('Ctrl Pts',(4.0965946873723,1.67945364446992,0.403489099757173));
#13003=CARTESIAN_POINT('Ctrl Pts',(4.1,1.66887738702936,0.605315322680078));
#13004=CARTESIAN_POINT('Ctrl Pts',(5.36191629113061,1.76821426155324,6.25990704884337E-5));
#13005=CARTESIAN_POINT('Ctrl Pts',(5.3630514496163,1.75763653340724,0.201889184585558));
#13006=CARTESIAN_POINT('Ctrl Pts',(5.36418670607087,1.74705878400967,0.403715765068683));
#13007=CARTESIAN_POINT('Ctrl Pts',(5.36532191986745,1.73648104871457,0.605542351516858));
#13008=CARTESIAN_POINT('Ctrl Pts',(6.63535348785608,1.76179300730897,3.38749616628245E-5));
#13009=CARTESIAN_POINT('Ctrl Pts',(6.63422081650235,1.75121562356675,0.20186041917081));
#13010=CARTESIAN_POINT('Ctrl Pts',(6.63308817234583,1.74063821462875,0.403686959568233));
#13011=CARTESIAN_POINT('Ctrl Pts',(6.63195543348166,1.7300608292057,0.605513504373875));
#13012=CARTESIAN_POINT('Ctrl Pts',(7.91019312949454,1.70715885937616,-0.000134060602928919));
#13013=CARTESIAN_POINT('Ctrl Pts',(7.90679525186394,1.69658223815078,0.201692207018782));
#13014=CARTESIAN_POINT('Ctrl Pts',(7.90339729485302,1.68600562209044,0.403518473580683));
#13015=CARTESIAN_POINT('Ctrl Pts',(7.89999925719352,1.67542901130525,0.605344739067286));
#13016=CARTESIAN_POINT('Origin',(3.9,1.7662962962963,0.));
#13017=CARTESIAN_POINT('',(3.9,-1.657567947596,0.605334330700044));
#13018=CARTESIAN_POINT('Ctrl Pts',(3.9,-1.657567947596,0.605334330700044));
#13019=CARTESIAN_POINT('Ctrl Pts',(3.9,-1.66295505583237,0.504667750148195));
#13020=CARTESIAN_POINT('Ctrl Pts',(3.9,-1.66834175427306,0.404000185805616));
#13021=CARTESIAN_POINT('Ctrl Pts',(3.9,-1.67913790341918,0.202222727053817));
#13022=CARTESIAN_POINT('Ctrl Pts',(3.9,-1.68454745406112,0.101110889248462));
#13023=CARTESIAN_POINT('Ctrl Pts',(3.9,-1.68995649764597,0.));
#13024=CARTESIAN_POINT('',(3.9,-1.55753217754889,0.7));
#13025=CARTESIAN_POINT('Ctrl Pts',(3.89999999700315,-1.55753217437,0.7));
#13026=CARTESIAN_POINT('Ctrl Pts',(3.89999999197785,-1.56545359401377,0.699999998841372));
#13027=CARTESIAN_POINT('Ctrl Pts',(3.90000117861029,-1.57331197233837,0.699006163267487));
#13028=CARTESIAN_POINT('Ctrl Pts',(3.90000221019459,-1.58096665047841,0.697118921400131));
#13029=CARTESIAN_POINT('Ctrl Pts',(3.90000279139136,-1.58527931230009,0.696055645348449));
#13030=CARTESIAN_POINT('Ctrl Pts',(3.90000331912093,-1.58952737074567,0.694707745526415));
#13031=CARTESIAN_POINT('Ctrl Pts',(3.90000364796674,-1.59368396010392,0.693086194530447));
#13032=CARTESIAN_POINT('Ctrl Pts',(3.90000423564848,-1.60111221870485,0.690188313817561));
#13033=CARTESIAN_POINT('Ctrl Pts',(3.90000407815102,-1.60816848972648,0.686450841450731));
#13034=CARTESIAN_POINT('Ctrl Pts',(3.9000032813392,-1.6147063365644,0.681954558458482));
#13035=CARTESIAN_POINT('Ctrl Pts',(3.90000284137901,-1.61831621321653,0.679471932695374));
#13036=CARTESIAN_POINT('Ctrl Pts',(3.90000222202081,-1.62176776859012,0.67675708350434));
#13037=CARTESIAN_POINT('Ctrl Pts',(3.9000016760669,-1.6250323621476,0.673818036286869));
#13038=CARTESIAN_POINT('Ctrl Pts',(3.90000114791654,-1.62819049732732,0.670974831382826));
#13039=CARTESIAN_POINT('Ctrl Pts',(3.90000068451114,-1.63115458712464,0.667938911589952));
#13040=CARTESIAN_POINT('Ctrl Pts',(3.90000068976928,-1.6339023205034,0.664721489040691));
#13041=CARTESIAN_POINT('Ctrl Pts',(3.90000069956116,-1.63901923218135,0.658729908073458));
#13042=CARTESIAN_POINT('Ctrl Pts',(3.9000021571807,-1.64338878348726,0.652110283780478));
#13043=CARTESIAN_POINT('Ctrl Pts',(3.90000267296827,-1.64695081636755,0.645027851744832));
#13044=CARTESIAN_POINT('Ctrl Pts',(3.90000272641596,-1.64731992654249,0.644293945625623));
#13045=CARTESIAN_POINT('Ctrl Pts',(3.90000277224081,-1.64768032438231,0.643555049900053));
#13046=CARTESIAN_POINT('Ctrl Pts',(3.90000280957334,-1.64803191324525,0.642811337026806));
#13047=CARTESIAN_POINT('Ctrl Pts',(3.90000316967295,-1.65142324611312,0.635637680016741));
#13048=CARTESIAN_POINT('Ctrl Pts',(3.90000247513984,-1.65395957542788,0.628100801230905));
#13049=CARTESIAN_POINT('Ctrl Pts',(3.90000142932204,-1.65558732484325,0.62036898832433));
#13050=CARTESIAN_POINT('Ctrl Pts',(3.90000076044003,-1.65662839749185,0.615423891207338));
#13051=CARTESIAN_POINT('Ctrl Pts',(3.9,-1.65729694754734,0.61039839235075));
#13052=CARTESIAN_POINT('Ctrl Pts',(3.9,-1.657567947596,0.605334330700044));
#13053=CARTESIAN_POINT('',(3.9,1.55753217754922,0.7));
#13054=CARTESIAN_POINT('',(3.9,0.883148148148148,0.7));
#13055=CARTESIAN_POINT('',(3.9,1.657567947596,0.605334330700044));
#13056=CARTESIAN_POINT('Ctrl Pts',(3.9,1.657567947596,0.605334330700044));
#13057=CARTESIAN_POINT('Ctrl Pts',(3.9,1.65714453107083,0.613246533660879));
#13058=CARTESIAN_POINT('Ctrl Pts',(3.90000169450566,1.65575314729854,0.621067109624563));
#13059=CARTESIAN_POINT('Ctrl Pts',(3.900002426785,1.653477907766,0.628635640467799));
#13060=CARTESIAN_POINT('Ctrl Pts',(3.90000283370343,1.65221358571927,0.632841378048222));
#13061=CARTESIAN_POINT('Ctrl Pts',(3.90000300372053,1.65067534627202,0.636969322077829));
#13062=CARTESIAN_POINT('Ctrl Pts',(3.90000288278183,1.6488710006323,0.640990000951852));
#13063=CARTESIAN_POINT('Ctrl Pts',(3.90000266510116,1.6456233127241,0.64822692378658));
#13064=CARTESIAN_POINT('Ctrl Pts',(3.90000136145047,1.64155197609259,0.655037842274187));
#13065=CARTESIAN_POINT('Ctrl Pts',(3.9000008487987,1.63672139510901,0.661259788874982));
#13066=CARTESIAN_POINT('Ctrl Pts',(3.90000075195303,1.63580884415802,0.662435184403355));
#13067=CARTESIAN_POINT('Ctrl Pts',(3.90000069125178,1.63486906637168,0.663589490553999));
#13068=CARTESIAN_POINT('Ctrl Pts',(3.90000068992127,1.63390232051248,0.664721489040685));
#13069=CARTESIAN_POINT('Ctrl Pts',(3.90000068733544,1.63202347103487,0.666921503393101));
#13070=CARTESIAN_POINT('Ctrl Pts',(3.9000009071255,1.6300427915863,0.669037305429552));
#13071=CARTESIAN_POINT('Ctrl Pts',(3.90000121037842,1.62796736695056,0.671065303566633));
#13072=CARTESIAN_POINT('Ctrl Pts',(3.90000204102081,1.62228255539437,0.676620208836154));
#13073=CARTESIAN_POINT('Ctrl Pts',(3.90000335328325,1.61595386407616,0.681456575151491));
#13074=CARTESIAN_POINT('Ctrl Pts',(3.90000380482706,1.60914557515952,0.685520902406533));
#13075=CARTESIAN_POINT('Ctrl Pts',(3.90000409284089,1.60480295930069,0.688113302965514));
#13076=CARTESIAN_POINT('Ctrl Pts',(3.90000408819389,1.6002642541482,0.690390927291682));
#13077=CARTESIAN_POINT('Ctrl Pts',(3.90000378365133,1.59556629223371,0.692330537597694));
#13078=CARTESIAN_POINT('Ctrl Pts',(3.90000330864444,1.58823869807682,0.695355823328757));
#13079=CARTESIAN_POINT('Ctrl Pts',(3.90000209726118,1.58060840086481,0.697526456028474));
#13080=CARTESIAN_POINT('Ctrl Pts',(3.90000112250675,1.5728228815436,0.698773197673241));
#13081=CARTESIAN_POINT('Ctrl Pts',(3.90000049100668,1.56777898966077,0.699580906164169));
#13082=CARTESIAN_POINT('Ctrl Pts',(3.89999999374416,1.56266934880282,0.69999999924861));
#13083=CARTESIAN_POINT('Ctrl Pts',(3.89999999700315,1.55753217437,0.7));
#13084=CARTESIAN_POINT('Ctrl Pts',(3.9,1.68995649764597,0.));
#13085=CARTESIAN_POINT('Ctrl Pts',(3.9,1.68454744095908,0.101111134163871));
#13086=CARTESIAN_POINT('Ctrl Pts',(3.9,1.67913787721413,0.202223216861756));
#13087=CARTESIAN_POINT('Ctrl Pts',(3.9,1.66834172806373,0.404000675610066));
#13088=CARTESIAN_POINT('Ctrl Pts',(3.9,1.66295504272671,0.504667995047933));
#13089=CARTESIAN_POINT('Ctrl Pts',(3.9,1.657567947596,0.605334330700044));
#13090=CARTESIAN_POINT('Ctrl Pts',(3.90000000000029,-1.68995649764598,2.25514051876985E-17));
#13091=CARTESIAN_POINT('Ctrl Pts',(3.90375240214247,-1.67935614215062,0.202290156525516));
#13092=CARTESIAN_POINT('Ctrl Pts',(3.90750491350916,-1.66875579641967,0.404580311547879));
#13093=CARTESIAN_POINT('Ctrl Pts',(3.91125753584366,-1.65815546066147,0.606870465045848));
#13094=CARTESIAN_POINT('Ctrl Pts',(2.95719731373254,-1.63434162994996,-0.000186284957671625));
#13095=CARTESIAN_POINT('Ctrl Pts',(2.96263618266967,-1.62374249289717,0.202103577800055));
#13096=CARTESIAN_POINT('Ctrl Pts',(2.96807524459186,-1.6131433886527,0.404393433349269));
#13097=CARTESIAN_POINT('Ctrl Pts',(2.97351444051957,-1.60254429060724,0.606683290324339));
#13098=CARTESIAN_POINT('Ctrl Pts',(2.0151035222252,-1.5373601393942,-0.000515615972119944));
#13099=CARTESIAN_POINT('Ctrl Pts',(2.0222299762717,-1.52676329064944,0.20177372753372));
#13100=CARTESIAN_POINT('Ctrl Pts',(2.02935668076532,-1.51616649670304,0.404063061036967));
#13101=CARTESIAN_POINT('Ctrl Pts',(2.03648357820815,-1.50556972342972,0.606352393906678));
#13102=CARTESIAN_POINT('Ctrl Pts',(1.07355614839761,-1.3885225322474,-0.00102014041634142));
#13103=CARTESIAN_POINT('Ctrl Pts',(1.08237048982668,-1.37792954541675,0.201268457136957));
#13104=CARTESIAN_POINT('Ctrl Pts',(1.09118510562603,-1.36733662501784,0.403557046289628));
#13105=CARTESIAN_POINT('Ctrl Pts',(1.09999999998551,-1.35674377243019,0.605845626932519));
#13106=CARTESIAN_POINT('Ctrl Pts',(1.10000000359112,-1.35674374984279,0.605845627045242));
#13107=CARTESIAN_POINT('Ctrl Pts',(2.02777573897866,-1.50422778688462,0.60559460123127));
#13108=CARTESIAN_POINT('Ctrl Pts',(2.96295221054883,-1.60165319397541,0.605428415101273));
#13109=CARTESIAN_POINT('Ctrl Pts',(3.9,-1.657567947596,0.605334330700044));
#13110=CARTESIAN_POINT('Ctrl Pts',(3.90594750914669,-1.55788759822396,0.7));
#13111=CARTESIAN_POINT('Ctrl Pts',(2.96654482017732,-1.50183737247472,0.7));
#13112=CARTESIAN_POINT('Ctrl Pts',(2.02939151553635,-1.40396309164617,0.7));
#13113=CARTESIAN_POINT('Ctrl Pts',(1.1,-1.25565664448621,0.7));
#13114=CARTESIAN_POINT('Ctrl Pts',(3.90422602671531,-1.58673967158186,0.7));
#13115=CARTESIAN_POINT('Ctrl Pts',(2.9639697519154,-1.53062009474021,0.699999324449154));
#13116=CARTESIAN_POINT('Ctrl Pts',(2.02587169016863,-1.43262076012027,0.700001792708215));
#13117=CARTESIAN_POINT('Ctrl Pts',(1.09546090287069,-1.28410178925883,0.700000000000001));
#13118=CARTESIAN_POINT('Ctrl Pts',(3.90124198563808,-1.6367522482393,0.676652244116846));
#13119=CARTESIAN_POINT('Ctrl Pts',(2.95951584878018,-1.58051528054544,0.676683243227538));
#13120=CARTESIAN_POINT('Ctrl Pts',(2.01975879699698,-1.48229505764113,0.676737195552829));
#13121=CARTESIAN_POINT('Ctrl Pts',(1.08759175402576,-1.33341535796084,0.676819902351873));
#13122=CARTESIAN_POINT('Ctrl Pts',(3.90006887217438,-1.65641364884095,0.626981005337021));
#13123=CARTESIAN_POINT('Ctrl Pts',(2.95775794493813,-1.6001648299169,0.627061170854983));
#13124=CARTESIAN_POINT('Ctrl Pts',(2.01735267249256,-1.50192280897576,0.627202240820629));
#13125=CARTESIAN_POINT('Ctrl Pts',(1.08446813262788,-1.35299014570964,0.627416665943555));
#13126=CARTESIAN_POINT('Ctrl Pts',(3.9,-1.657567947596,0.605334330700044));
#13127=CARTESIAN_POINT('Ctrl Pts',(2.95765589353472,-1.60133715645388,0.605428946878649));
#13128=CARTESIAN_POINT('Ctrl Pts',(2.01720431860088,-1.50312513840151,0.605596482146283));
#13129=CARTESIAN_POINT('Ctrl Pts',(1.0842689834292,-1.35423815332579,0.605849891671036));
#13130=CARTESIAN_POINT('Ctrl Pts',(3.89999999700313,-1.55753217437,0.7));
#13131=CARTESIAN_POINT('Ctrl Pts',(2.96258932077475,-1.50142404037792,0.7));
#13132=CARTESIAN_POINT('Ctrl Pts',(2.02743012901897,-1.40365010593343,0.7));
#13133=CARTESIAN_POINT('Ctrl Pts',(1.1,-1.25565664448621,0.7));
#13134=CARTESIAN_POINT('Origin',(6.08012166120517,1.06778195214465E-16,
0.7));
#13135=CARTESIAN_POINT('Ctrl Pts',(1.1,1.25565664448621,0.7));
#13136=CARTESIAN_POINT('Ctrl Pts',(2.02743012901899,1.40365010593344,0.7));
#13137=CARTESIAN_POINT('Ctrl Pts',(2.96258932077472,1.50142404037792,0.7));
#13138=CARTESIAN_POINT('Ctrl Pts',(3.89999999700315,1.55753217437,0.7));
#13139=CARTESIAN_POINT('Ctrl Pts',(1.1,1.25565664448621,0.7));
#13140=CARTESIAN_POINT('Ctrl Pts',(2.02939151553637,1.40396309164617,0.7));
#13141=CARTESIAN_POINT('Ctrl Pts',(2.96654482017727,1.50183737247472,0.7));
#13142=CARTESIAN_POINT('Ctrl Pts',(3.90594750914669,1.55788759822396,0.7));
#13143=CARTESIAN_POINT('Ctrl Pts',(1.09546090287069,1.28410178925883,0.700000000000001));
#13144=CARTESIAN_POINT('Ctrl Pts',(2.02587169016866,1.43262076012027,0.700001792708215));
#13145=CARTESIAN_POINT('Ctrl Pts',(2.96396975191535,1.53062009474021,0.699999324449154));
#13146=CARTESIAN_POINT('Ctrl Pts',(3.90422602671531,1.58673967158186,0.7));
#13147=CARTESIAN_POINT('Ctrl Pts',(1.08759175402576,1.33341535796084,0.676819902351873));
#13148=CARTESIAN_POINT('Ctrl Pts',(2.019758796997,1.48229505764113,0.676737195552829));
#13149=CARTESIAN_POINT('Ctrl Pts',(2.95951584878014,1.58051528054544,0.676683243227538));
#13150=CARTESIAN_POINT('Ctrl Pts',(3.90124198563808,1.6367522482393,0.676652244116846));
#13151=CARTESIAN_POINT('Ctrl Pts',(1.08446813262788,1.35299014570964,0.627416665943555));
#13152=CARTESIAN_POINT('Ctrl Pts',(2.01735267249258,1.50192280897576,0.627202240820629));
#13153=CARTESIAN_POINT('Ctrl Pts',(2.95775794493809,1.6001648299169,0.627061170854983));
#13154=CARTESIAN_POINT('Ctrl Pts',(3.90006887217438,1.65641364884095,0.626981005337021));
#13155=CARTESIAN_POINT('Ctrl Pts',(1.0842689834292,1.35423815332579,0.605849891671036));
#13156=CARTESIAN_POINT('Ctrl Pts',(2.0172043186009,1.50312513840152,0.605596482146283));
#13157=CARTESIAN_POINT('Ctrl Pts',(2.95765589353468,1.60133715645387,0.605428946878649));
#13158=CARTESIAN_POINT('Ctrl Pts',(3.9,1.657567947596,0.605334330700044));
#13159=CARTESIAN_POINT('Ctrl Pts',(3.9,1.657567947596,0.605334330700044));
#13160=CARTESIAN_POINT('Ctrl Pts',(2.96295221054879,1.60165319397541,0.605428415101273));
#13161=CARTESIAN_POINT('Ctrl Pts',(2.02777573897867,1.50422778688462,0.60559460123127));
#13162=CARTESIAN_POINT('Ctrl Pts',(1.10000000359111,1.35674374984279,0.605845627045242));
#13163=CARTESIAN_POINT('Ctrl Pts',(1.07355614839761,1.3885225322474,-0.00102014041634139));
#13164=CARTESIAN_POINT('Ctrl Pts',(1.08237048982668,1.37792954541676,0.201268457136957));
#13165=CARTESIAN_POINT('Ctrl Pts',(1.09118510562602,1.36733662501784,0.403557046289628));
#13166=CARTESIAN_POINT('Ctrl Pts',(1.09999999998551,1.35674377243019,0.605845626932519));
#13167=CARTESIAN_POINT('Ctrl Pts',(2.0151035222252,1.5373601393942,-0.000515615972119942));
#13168=CARTESIAN_POINT('Ctrl Pts',(2.0222299762717,1.52676329064944,0.201773727533721));
#13169=CARTESIAN_POINT('Ctrl Pts',(2.02935668076532,1.51616649670304,0.404063061036968));
#13170=CARTESIAN_POINT('Ctrl Pts',(2.03648357820815,1.50556972342972,0.606352393906678));
#13171=CARTESIAN_POINT('Ctrl Pts',(2.95719731373254,1.63434162994996,-0.000186284957671606));
#13172=CARTESIAN_POINT('Ctrl Pts',(2.96263618266967,1.62374249289717,0.202103577800055));
#13173=CARTESIAN_POINT('Ctrl Pts',(2.96807524459186,1.6131433886527,0.404393433349269));
#13174=CARTESIAN_POINT('Ctrl Pts',(2.97351444051957,1.60254429060724,0.60668329032434));
#13175=CARTESIAN_POINT('Ctrl Pts',(3.90000000000029,1.68995649764598,4.33680868994202E-17));
#13176=CARTESIAN_POINT('Ctrl Pts',(3.90375240214247,1.67935614215062,0.202290156525516));
#13177=CARTESIAN_POINT('Ctrl Pts',(3.90750491350917,1.66875579641967,0.404580311547879));
#13178=CARTESIAN_POINT('Ctrl Pts',(3.91125753584366,1.65815546066147,0.606870465045848));
#13179=CARTESIAN_POINT('Origin',(0.9,1.44962962962963,0.));
#13180=CARTESIAN_POINT('',(0.900000000000025,-1.32415632515176,0.605901073595307));
#13181=CARTESIAN_POINT('Ctrl Pts',(0.900000000000025,-1.32415632515176,
0.605901073595307));
#13182=CARTESIAN_POINT('Ctrl Pts',(0.900000000000025,-1.33021622058432,
0.504787384877132));
#13183=CARTESIAN_POINT('Ctrl Pts',(0.900000000000001,-1.33627289299046,
0.403672458220672));
#13184=CARTESIAN_POINT('Ctrl Pts',(0.900000000000001,-1.3483639425303,0.201706128802639));
#13185=CARTESIAN_POINT('Ctrl Pts',(0.9,-1.3543984610184,0.100852646477479));
#13186=CARTESIAN_POINT('Ctrl Pts',(0.9,-1.3604297237941,0.));
#13187=CARTESIAN_POINT('',(0.9,-1.22294421121193,0.7));
#13188=CARTESIAN_POINT('Ctrl Pts',(0.899999998934589,-1.2229442093848,0.7));
#13189=CARTESIAN_POINT('Ctrl Pts',(0.89999998269596,-1.2309559991361,0.699999991698178));
#13190=CARTESIAN_POINT('Ctrl Pts',(0.900003161357076,-1.2389110096839,0.699008412490225));
#13191=CARTESIAN_POINT('Ctrl Pts',(0.900005837532895,-1.24666554379878,
0.697120920272419));
#13192=CARTESIAN_POINT('Ctrl Pts',(0.900007138246235,-1.25043451364619,
0.69620353424371));
#13193=CARTESIAN_POINT('Ctrl Pts',(0.900008321383585,-1.25415610217771,
0.695073675615989));
#13194=CARTESIAN_POINT('Ctrl Pts',(0.900009136546862,-1.25781268161099,
0.69373809091454));
#13195=CARTESIAN_POINT('Ctrl Pts',(0.90001081442992,-1.26533916477404,0.690989003700189));
#13196=CARTESIAN_POINT('Ctrl Pts',(0.900010659344479,-1.27251458345821,
0.687399440976464));
#13197=CARTESIAN_POINT('Ctrl Pts',(0.900008585023094,-1.27919110928202,
0.68304500924512));
#13198=CARTESIAN_POINT('Ctrl Pts',(0.900007251085311,-1.28348459539356,
0.680244796581297));
#13199=CARTESIAN_POINT('Ctrl Pts',(0.900005156998288,-1.28757155292352,
0.67712723751572));
#13200=CARTESIAN_POINT('Ctrl Pts',(0.900003422242992,-1.29140570811059,
0.673703384872626));
#13201=CARTESIAN_POINT('Ctrl Pts',(0.90000203719427,-1.29446694202502,0.670969741262059));
#13202=CARTESIAN_POINT('Ctrl Pts',(0.90000088611098,-1.29734878548314,0.668056850549005));
#13203=CARTESIAN_POINT('Ctrl Pts',(0.900000936626746,-1.30003070819003,
0.664973821719563));
#13204=CARTESIAN_POINT('Ctrl Pts',(0.90000103432908,-1.30521780373233,0.659010948495488));
#13205=CARTESIAN_POINT('Ctrl Pts',(0.900005119671874,-1.30966005175478,
0.652412896960716));
#13206=CARTESIAN_POINT('Ctrl Pts',(0.900006662646281,-1.31329014967729,
0.64534035177384));
#13207=CARTESIAN_POINT('Ctrl Pts',(0.900006837929091,-1.31370253096037,
0.644536906434065));
#13208=CARTESIAN_POINT('Ctrl Pts',(0.900006988901759,-1.3141043809937,0.64372731654354));
#13209=CARTESIAN_POINT('Ctrl Pts',(0.900007112770807,-1.31449556093743,
0.642911804846506));
#13210=CARTESIAN_POINT('Ctrl Pts',(0.900008198175579,-1.31792328224658,
0.635765868899185));
#13211=CARTESIAN_POINT('Ctrl Pts',(0.900006415208278,-1.32049402672979,
0.628253543462219));
#13212=CARTESIAN_POINT('Ctrl Pts',(0.900003664797616,-1.32215034643222,
0.620540220943237));
#13213=CARTESIAN_POINT('Ctrl Pts',(0.900001948338234,-1.32318401225236,
0.615726538031782));
#13214=CARTESIAN_POINT('Ctrl Pts',(0.900000000000001,-1.32386068836271,
0.610833984830158));
#13215=CARTESIAN_POINT('Ctrl Pts',(0.900000000000001,-1.32415632515176,
0.605901073595307));
#13216=CARTESIAN_POINT('',(0.9,1.22294421121193,0.7));
#13217=CARTESIAN_POINT('',(0.9,0.724814814814815,0.7));
#13218=CARTESIAN_POINT('',(0.900000000000027,1.32415632515176,0.605901073595307));
#13219=CARTESIAN_POINT('Ctrl Pts',(0.900000000000001,1.32415632515176,0.605901073595307));
#13220=CARTESIAN_POINT('Ctrl Pts',(0.900000000000001,1.32368299187747,0.613798977756921));
#13221=CARTESIAN_POINT('Ctrl Pts',(0.900004523569871,1.32223544152535,0.621596324701597));
#13222=CARTESIAN_POINT('Ctrl Pts',(0.900006356724635,1.31990036466821,0.629134362570908));
#13223=CARTESIAN_POINT('Ctrl Pts',(0.900007328861843,1.3186620540024,0.633131846706937));
#13224=CARTESIAN_POINT('Ctrl Pts',(0.900007702029268,1.31717322147439,0.637056437951431));
#13225=CARTESIAN_POINT('Ctrl Pts',(0.900007358328755,1.31544117393516,0.640882963165587));
#13226=CARTESIAN_POINT('Ctrl Pts',(0.900006707239278,1.31216006761937,0.648131745755711));
#13227=CARTESIAN_POINT('Ctrl Pts',(0.900003091243194,1.3080468004769,0.654946293188228));
#13228=CARTESIAN_POINT('Ctrl Pts',(0.900001489347898,1.30317324258861,0.661167512355852));
#13229=CARTESIAN_POINT('Ctrl Pts',(0.900001155878064,1.30215870403359,0.662462596327245));
#13230=CARTESIAN_POINT('Ctrl Pts',(0.90000093695446,1.30111105636563,0.663731893727214));
#13231=CARTESIAN_POINT('Ctrl Pts',(0.90000091848414,1.30003070515708,0.664973821721807));
#13232=CARTESIAN_POINT('Ctrl Pts',(0.90000089007412,1.29836896897911,0.666884086330845));
#13233=CARTESIAN_POINT('Ctrl Pts',(0.900001333486324,1.29662987445651,0.668729618924651));
#13234=CARTESIAN_POINT('Ctrl Pts',(0.900001997973453,1.2948182721625,0.670508241825176));
#13235=CARTESIAN_POINT('Ctrl Pts',(0.900004083621534,1.28913213515815,0.676090865298813));
#13236=CARTESIAN_POINT('Ctrl Pts',(0.900007925915178,1.28279871831387,0.680954424681199));
#13237=CARTESIAN_POINT('Ctrl Pts',(0.900009431597099,1.27598654051802,0.685053039288488));
#13238=CARTESIAN_POINT('Ctrl Pts',(0.900010426918848,1.2714833923965,0.687762403198649));
#13239=CARTESIAN_POINT('Ctrl Pts',(0.900010579450444,1.26676996242859,0.690136867340003));
#13240=CARTESIAN_POINT('Ctrl Pts',(0.900009885932263,1.26188774903006,0.692153145632694));
#13241=CARTESIAN_POINT('Ctrl Pts',(0.900008832351734,1.25447077696631,0.695216239878874));
#13242=CARTESIAN_POINT('Ctrl Pts',(0.900005746465811,1.24674633448708,0.697421320974322));
#13243=CARTESIAN_POINT('Ctrl Pts',(0.900003140090462,1.23886595492982,0.6987028844583));
#13244=CARTESIAN_POINT('Ctrl Pts',(0.900001403206082,1.23361448254879,0.699556916322089));
#13245=CARTESIAN_POINT('Ctrl Pts',(0.899999988093253,1.22829309040712,0.699999994457486));
#13246=CARTESIAN_POINT('Ctrl Pts',(0.899999998934588,1.2229442093848,0.7));
#13247=CARTESIAN_POINT('Ctrl Pts',(0.9,1.3604297237941,0.));
#13248=CARTESIAN_POINT('Ctrl Pts',(0.9,1.35439838926384,0.100853846331769));
#13249=CARTESIAN_POINT('Ctrl Pts',(0.9,1.34836379894337,0.201708528537181));
#13250=CARTESIAN_POINT('Ctrl Pts',(0.9,1.33627274925098,0.403674857922336));
#13251=CARTESIAN_POINT('Ctrl Pts',(0.900000000000027,1.33021614867672,0.504788584706939));
#13252=CARTESIAN_POINT('Ctrl Pts',(0.900000000000027,1.32415632515176,0.605901073595307));
#13253=CARTESIAN_POINT('Ctrl Pts',(0.900000000000001,-1.3604297237941,-1.73472347597681E-18));
#13254=CARTESIAN_POINT('Ctrl Pts',(0.909119345746934,-1.34984469470005,
0.202150401646216));
#13255=CARTESIAN_POINT('Ctrl Pts',(0.918238975454288,-1.33925973741039,
0.404300794324169));
#13256=CARTESIAN_POINT('Ctrl Pts',(0.92735889343571,-1.32867485341111,0.606451177918334));
#13257=CARTESIAN_POINT('Ctrl Pts',(0.693791632045388,-1.32642527651154,
-0.000115194085079675));
#13258=CARTESIAN_POINT('Ctrl Pts',(0.703280422539661,-1.31584113310577,
0.202035038813999));
#13259=CARTESIAN_POINT('Ctrl Pts',(0.712769508818954,-1.30525706820637,
0.404185262036053));
#13260=CARTESIAN_POINT('Ctrl Pts',(0.722258895242942,-1.29467308328318,
0.606335475483814));
#13261=CARTESIAN_POINT('Ctrl Pts',(0.487608314405001,-1.28990207050556,
-0.000238777108575344));
#13262=CARTESIAN_POINT('Ctrl Pts',(0.497466558273561,-1.27931888757273,
0.201911276725417));
#13263=CARTESIAN_POINT('Ctrl Pts',(0.507325109482935,-1.26873579028159,
0.404061320158324));
#13264=CARTESIAN_POINT('Ctrl Pts',(0.517183972542757,-1.25815278023897,
0.606211353085106));
#13265=CARTESIAN_POINT('Ctrl Pts',(0.281447431601629,-1.2507496025167,-0.000370926150909055));
#13266=CARTESIAN_POINT('Ctrl Pts',(0.291675125201343,-1.24016745708839,
0.201778938960696));
#13267=CARTESIAN_POINT('Ctrl Pts',(0.301903137322998,-1.2295854048496,0.403928792940867));
#13268=CARTESIAN_POINT('Ctrl Pts',(0.312131472716966,-1.21900344770756,
0.606078635650713));
#13269=CARTESIAN_POINT('',(0.313137632044026,-1.21919552599285,0.606079286803921));
#13270=CARTESIAN_POINT('Ctrl Pts',(0.28146619846596,-1.25073018526678,-6.36968776335234E-17));
#13271=CARTESIAN_POINT('Ctrl Pts',(0.292023490345879,-1.2402182973453,0.20202640462578));
#13272=CARTESIAN_POINT('Ctrl Pts',(0.302580635585432,-1.22970674279184,
0.404052833452346));
#13273=CARTESIAN_POINT('Ctrl Pts',(0.313137632044028,-1.21919552599286,
0.606079286803922));
#13274=CARTESIAN_POINT('Ctrl Pts',(0.313137632044026,-1.21919552599285,
0.606079286803921));
#13275=CARTESIAN_POINT('Ctrl Pts',(0.508347756773358,-1.25646926692181,
0.606016122348466));
#13276=CARTESIAN_POINT('Ctrl Pts',(0.703992099548353,-1.29143758865737,
0.605956720831638));
#13277=CARTESIAN_POINT('Ctrl Pts',(0.900000000000031,-1.32415632515176,
0.605901073595307));
#13278=CARTESIAN_POINT('Ctrl Pts',(0.916434425702686,-1.22569269236154,
0.7));
#13279=CARTESIAN_POINT('Ctrl Pts',(0.72117838049967,-1.193102781986,0.7));
#13280=CARTESIAN_POINT('Ctrl Pts',(0.526295996270969,-1.15827411715321,
0.7));
#13281=CARTESIAN_POINT('Ctrl Pts',(0.3318563713692,-1.12115139781564,0.7));
#13282=CARTESIAN_POINT('Ctrl Pts',(0.911693828447622,-1.25409504944868,
0.700000000000001));
#13283=CARTESIAN_POINT('Ctrl Pts',(0.716221724293519,-1.22145811194286,
0.699999606692487));
#13284=CARTESIAN_POINT('Ctrl Pts',(0.52112301919326,-1.18657973614434,0.700000445015345));
#13285=CARTESIAN_POINT('Ctrl Pts',(0.32646265058614,-1.14940237362229,0.699999999999999));
#13286=CARTESIAN_POINT('Ctrl Pts',(0.903473253113197,-1.30334701150065,
0.676847307332805));
#13287=CARTESIAN_POINT('Ctrl Pts',(0.707628846166824,-1.27063023858114,
0.676865462359186));
#13288=CARTESIAN_POINT('Ctrl Pts',(0.512149925983835,-1.23566412474798,
0.676884474751893));
#13289=CARTESIAN_POINT('Ctrl Pts',(0.317109102097966,-1.19839394783867,
0.676905055067496));
#13290=CARTESIAN_POINT('Ctrl Pts',(0.900209809599689,-1.32289929215588,
0.627459885485154));
#13291=CARTESIAN_POINT('Ctrl Pts',(0.704212910592823,-1.29017057588713,
0.627506965865002));
#13292=CARTESIAN_POINT('Ctrl Pts',(0.50858160780484,-1.25519230329596,0.627556915196293));
#13293=CARTESIAN_POINT('Ctrl Pts',(0.31338355686088,-1.21790743260971,0.627610331402299));
#13294=CARTESIAN_POINT('Ctrl Pts',(0.900000000000031,-1.32415632515176,
0.605901073595307));
#13295=CARTESIAN_POINT('Ctrl Pts',(0.703992099548353,-1.29143758865737,
0.605956720831638));
#13296=CARTESIAN_POINT('Ctrl Pts',(0.508347756773358,-1.25646926692181,
0.606016122348466));
#13297=CARTESIAN_POINT('Ctrl Pts',(0.313137632044026,-1.21919552599285,
0.606079286803921));
#13298=CARTESIAN_POINT('',(0.3318563713692,-1.12115139781563,0.7));
#13299=CARTESIAN_POINT('Origin',(0.331856371369202,-1.12115139781563,0.6));
#13300=CARTESIAN_POINT('Ctrl Pts',(0.899999998934586,-1.2229442093848,0.7));
#13301=CARTESIAN_POINT('Ctrl Pts',(0.71024282334811,-1.19114655107378,0.7));
#13302=CARTESIAN_POINT('Ctrl Pts',(0.520840466228891,-1.15723253876768,
0.7));
#13303=CARTESIAN_POINT('Ctrl Pts',(0.3318563713692,-1.12115139781564,0.7));
#13304=CARTESIAN_POINT('Origin',(6.08012166120517,1.06778195214465E-16,
0.7));
#13305=CARTESIAN_POINT('',(0.331856371369203,1.12115139781563,0.7));
#13306=CARTESIAN_POINT('',(0.3318563713692,-0.7,0.7));
#13307=CARTESIAN_POINT('Ctrl Pts',(0.331856371369202,1.12115139781564,0.7));
#13308=CARTESIAN_POINT('Ctrl Pts',(0.520840466228894,1.15723253876768,0.7));
#13309=CARTESIAN_POINT('Ctrl Pts',(0.710242823348114,1.19114655107378,0.7));
#13310=CARTESIAN_POINT('Ctrl Pts',(0.899999998934589,1.2229442093848,0.7));
#13311=CARTESIAN_POINT('Ctrl Pts',(0.281447431601628,1.2507496025167,-0.000370926150909064));
#13312=CARTESIAN_POINT('Ctrl Pts',(0.291675125201342,1.24016745708839,0.201778938960695));
#13313=CARTESIAN_POINT('Ctrl Pts',(0.301903137322998,1.2295854048496,0.403928792940867));
#13314=CARTESIAN_POINT('Ctrl Pts',(0.312131472716965,1.21900344770756,0.606078635650713));
#13315=CARTESIAN_POINT('Ctrl Pts',(0.487608314405001,1.28990207050556,-0.000238777108575355));
#13316=CARTESIAN_POINT('Ctrl Pts',(0.497466558273561,1.27931888757273,0.201911276725417));
#13317=CARTESIAN_POINT('Ctrl Pts',(0.507325109482935,1.26873579028159,0.404061320158324));
#13318=CARTESIAN_POINT('Ctrl Pts',(0.517183972542757,1.25815278023897,0.606211353085106));
#13319=CARTESIAN_POINT('Ctrl Pts',(0.693791632045388,1.32642527651154,-0.000115194085079627));
#13320=CARTESIAN_POINT('Ctrl Pts',(0.703280422539661,1.31584113310577,0.202035038813999));
#13321=CARTESIAN_POINT('Ctrl Pts',(0.712769508818955,1.30525706820637,0.404185262036054));
#13322=CARTESIAN_POINT('Ctrl Pts',(0.722258895242942,1.29467308328318,0.606335475483814));
#13323=CARTESIAN_POINT('Ctrl Pts',(0.900000000000002,1.3604297237941,4.33680868994202E-17));
#13324=CARTESIAN_POINT('Ctrl Pts',(0.909119345746935,1.34984469470005,0.202150401646216));
#13325=CARTESIAN_POINT('Ctrl Pts',(0.918238975454289,1.33925973741039,0.40430079432417));
#13326=CARTESIAN_POINT('Ctrl Pts',(0.927358893435711,1.32867485341111,0.606451177918334));
#13327=CARTESIAN_POINT('',(0.313137632044028,1.21919552599286,0.606079286803921));
#13328=CARTESIAN_POINT('Ctrl Pts',(0.900000000000026,1.32415632515176,0.605901073595307));
#13329=CARTESIAN_POINT('Ctrl Pts',(0.703992099548352,1.29143758865737,0.605956720831638));
#13330=CARTESIAN_POINT('Ctrl Pts',(0.508347756773358,1.25646926692181,0.606016122348466));
#13331=CARTESIAN_POINT('Ctrl Pts',(0.313137632044028,1.21919552599286,0.606079286803921));
#13332=CARTESIAN_POINT('Ctrl Pts',(0.313137632044028,1.21919552599286,0.606079286803922));
#13333=CARTESIAN_POINT('Ctrl Pts',(0.302580635585432,1.22970674279184,0.404052833452346));
#13334=CARTESIAN_POINT('Ctrl Pts',(0.29202349034588,1.2402182973453,0.20202640462578));
#13335=CARTESIAN_POINT('Ctrl Pts',(0.28146619846596,1.25073018526678,-6.5594231435373E-18));
#13336=CARTESIAN_POINT('Ctrl Pts',(0.331856371369202,1.12115139781564,0.7));
#13337=CARTESIAN_POINT('Ctrl Pts',(0.526295996270969,1.15827411715321,0.7));
#13338=CARTESIAN_POINT('Ctrl Pts',(0.72117838049967,1.193102781986,0.7));
#13339=CARTESIAN_POINT('Ctrl Pts',(0.916434425702682,1.22569269236154,0.7));
#13340=CARTESIAN_POINT('Ctrl Pts',(0.326462650586141,1.14940237362229,0.699999999999999));
#13341=CARTESIAN_POINT('Ctrl Pts',(0.52112301919326,1.18657973614434,0.700000445015345));
#13342=CARTESIAN_POINT('Ctrl Pts',(0.716221724293519,1.22145811194286,0.699999606692487));
#13343=CARTESIAN_POINT('Ctrl Pts',(0.911693828447618,1.25409504944868,0.700000000000001));
#13344=CARTESIAN_POINT('Ctrl Pts',(0.317109102097967,1.19839394783867,0.676905055067496));
#13345=CARTESIAN_POINT('Ctrl Pts',(0.512149925983836,1.23566412474798,0.676884474751893));
#13346=CARTESIAN_POINT('Ctrl Pts',(0.707628846166824,1.27063023858114,0.676865462359185));
#13347=CARTESIAN_POINT('Ctrl Pts',(0.903473253113193,1.30334701150065,0.676847307332805));
#13348=CARTESIAN_POINT('Ctrl Pts',(0.313383556860882,1.21790743260971,0.627610331402299));
#13349=CARTESIAN_POINT('Ctrl Pts',(0.508581607804839,1.25519230329596,0.627556915196293));
#13350=CARTESIAN_POINT('Ctrl Pts',(0.704212910592822,1.29017057588713,0.627506965865002));
#13351=CARTESIAN_POINT('Ctrl Pts',(0.900209809599685,1.32289929215587,0.627459885485154));
#13352=CARTESIAN_POINT('Ctrl Pts',(0.313137632044028,1.21919552599286,0.606079286803921));
#13353=CARTESIAN_POINT('Ctrl Pts',(0.508347756773358,1.25646926692181,0.606016122348466));
#13354=CARTESIAN_POINT('Ctrl Pts',(0.703992099548352,1.29143758865737,0.605956720831638));
#13355=CARTESIAN_POINT('Ctrl Pts',(0.900000000000026,1.32415632515176,0.605901073595307));
#13356=CARTESIAN_POINT('Origin',(0.3318563713692,1.12115139781563,0.6));
#13357=CARTESIAN_POINT('Origin',(0.3318563713692,1.12115139781563,0.6));
#13358=CARTESIAN_POINT('Origin',(0.3318563713692,1.12115139781563,0.6));
#13359=CARTESIAN_POINT('Origin',(0.331856371369201,1.12115139781563,0.6));
#13360=CARTESIAN_POINT('Origin',(11.6681436286308,1.2964346619681,0.6));
#13361=CARTESIAN_POINT('Origin',(11.6681436286308,1.2964346619681,0.6));
#13362=CARTESIAN_POINT('',(11.7680065821063,1.2964346619681,0.605233595624295));
#13363=CARTESIAN_POINT('Origin',(11.6681436286308,1.2964346619681,0.6));
#13364=CARTESIAN_POINT('Origin',(11.6681436286308,1.2964346619681,0.6));
#13365=CARTESIAN_POINT('Origin',(0.3318563713692,-1.12115139781563,0.6));
#13366=CARTESIAN_POINT('Origin',(0.3318563713692,-1.12115139781563,0.6));
#13367=CARTESIAN_POINT('Origin',(0.3318563713692,-1.12115139781563,0.6));
#13368=CARTESIAN_POINT('Origin',(0.3318563713692,-0.7,0.6));
#13369=CARTESIAN_POINT('Ctrl Pts',(0.281398851089427,-1.25079724300364,
-0.00128877254616805));
#13370=CARTESIAN_POINT('Ctrl Pts',(0.291978592719145,-1.24026300108396,
0.201167222825305));
#13371=CARTESIAN_POINT('Ctrl Pts',(0.302558187088771,-1.2297290939422,0.403623242499903));
#13372=CARTESIAN_POINT('Ctrl Pts',(0.313137632044028,-1.21919552599286,
0.606079286803922));
#13373=CARTESIAN_POINT('Ctrl Pts',(0.258825925396095,-1.24645021448495,
-0.000331836826913007));
#13374=CARTESIAN_POINT('Ctrl Pts',(0.269412087408768,-1.23590982471973,
0.202123507634926));
#13375=CARTESIAN_POINT('Ctrl Pts',(0.279998097240749,-1.22537010804418,
0.404578894752494));
#13376=CARTESIAN_POINT('Ctrl Pts',(0.290584031570127,-1.21483034200885,
0.60703428203898));
#13377=CARTESIAN_POINT('Ctrl Pts',(0.216858515231733,-1.22156435206688,
0.000573427186746937));
#13378=CARTESIAN_POINT('Ctrl Pts',(0.22746089442761,-1.21102065820065,0.20302778119957));
#13379=CARTESIAN_POINT('Ctrl Pts',(0.238063405890532,-1.20047706879609,
0.405482132943502));
#13380=CARTESIAN_POINT('Ctrl Pts',(0.248665715176951,-1.18993398276804,
0.607936521147589));
#13381=CARTESIAN_POINT('Ctrl Pts',(0.20022524016831,-1.1757120364715,-0.000939345874739115));
#13382=CARTESIAN_POINT('Ctrl Pts',(0.210835545796271,-1.16517845930889,
0.201515175954065));
#13383=CARTESIAN_POINT('Ctrl Pts',(0.221445511453644,-1.15464532122135,
0.403969738345816));
#13384=CARTESIAN_POINT('Ctrl Pts',(0.232055819885544,-1.1441124535127,0.606424296559432));
#13385=CARTESIAN_POINT('Ctrl Pts',(0.200162791320387,-1.15273540576203,
-0.00213094087794781));
#13386=CARTESIAN_POINT('Ctrl Pts',(0.210772999146098,-1.14220702337553,
0.200323884929633));
#13387=CARTESIAN_POINT('Ctrl Pts',(0.221383207999129,-1.13167901896849,
0.402778730339676));
#13388=CARTESIAN_POINT('Ctrl Pts',(0.231993417893744,-1.12115139781563,
0.605233595624295));
#13389=CARTESIAN_POINT('Origin',(11.6681436286308,-1.2964346619681,0.6));
#13390=CARTESIAN_POINT('',(11.7680065821063,-1.2964346619681,0.605233595624295));
#13391=CARTESIAN_POINT('Origin',(11.6681436286308,-1.2964346619681,0.6));
#13392=CARTESIAN_POINT('Origin',(11.6681436286308,-1.2964346619681,0.6));
#13393=CARTESIAN_POINT('Origin',(11.6681436286308,0.8,0.6));
#13394=CARTESIAN_POINT('',(11.7680065821063,0.8,0.605233595624295));
#13395=CARTESIAN_POINT('Ctrl Pts',(11.7998406965532,-1.32812796269332,-0.00219749346969486));
#13396=CARTESIAN_POINT('Ctrl Pts',(11.7892293257052,-1.31756329650235,0.200279524124498));
#13397=CARTESIAN_POINT('Ctrl Pts',(11.778617954226,-1.30699886176745,0.402756553762325));
#13398=CARTESIAN_POINT('Ctrl Pts',(11.7680065821063,-1.2964346619681,0.605233595624295));
#13399=CARTESIAN_POINT('Ctrl Pts',(11.7997644051931,-1.35610429277321,-0.000741767599518841));
#13400=CARTESIAN_POINT('Ctrl Pts',(11.7891529352516,-1.34553639595159,0.201735054786578));
#13401=CARTESIAN_POINT('Ctrl Pts',(11.7785417923834,-1.33496887357233,0.404211913913734));
#13402=CARTESIAN_POINT('Ctrl Pts',(11.7679303202531,-1.32440140973518,0.606688758469115));
#13403=CARTESIAN_POINT('Ctrl Pts',(11.777798894316,-1.40464673224301,0.000639873095493681));
#13404=CARTESIAN_POINT('Ctrl Pts',(11.7671928076068,-1.39407357725403,0.203116666245104));
#13405=CARTESIAN_POINT('Ctrl Pts',(11.7565866683578,-1.38350056680667,0.405593463707878));
#13406=CARTESIAN_POINT('Ctrl Pts',(11.7459806329718,-1.37292778989405,0.608070278434593));
#13407=CARTESIAN_POINT('Ctrl Pts',(11.7305637688674,-1.42539741767755,-0.000752904078362463));
#13408=CARTESIAN_POINT('Ctrl Pts',(11.7199663219939,-1.4148278080644,0.201724510929383));
#13409=CARTESIAN_POINT('Ctrl Pts',(11.7093688723049,-1.40425849106451,0.404201940657439));
#13410=CARTESIAN_POINT('Ctrl Pts',(11.6987715660822,-1.39368929079062,0.606679383299034));
#13411=CARTESIAN_POINT('Ctrl Pts',(11.7096810564041,-1.4274931182575,-0.0017379730583696));
#13412=CARTESIAN_POINT('Ctrl Pts',(11.6990862989954,-1.41692678914967,0.200739752511227));
#13413=CARTESIAN_POINT('Ctrl Pts',(11.6884916259906,-1.40636067879325,0.403217493356832));
#13414=CARTESIAN_POINT('Ctrl Pts',(11.6778970386953,-1.39579479040469,0.605695249702977));
#13415=CARTESIAN_POINT('Ctrl Pts',(11.7997255308004,-1.32801330383774,1.58293517182884E-17));
#13416=CARTESIAN_POINT('Ctrl Pts',(11.7891525485321,-1.31748685893698,0.201744519857947));
#13417=CARTESIAN_POINT('Ctrl Pts',(11.7785795656372,-1.30696064383315,0.403489051673192));
#13418=CARTESIAN_POINT('Ctrl Pts',(11.7680065821063,-1.2964346619681,0.605233595624295));
#13419=CARTESIAN_POINT('Ctrl Pts',(11.7096782931395,1.42749036240749,-0.00168516396645821));
#13420=CARTESIAN_POINT('Ctrl Pts',(11.6990844568337,1.41692495195436,0.200774958575157));
#13421=CARTESIAN_POINT('Ctrl Pts',(11.6884907049172,1.40635976021489,0.403235096390144));
#13422=CARTESIAN_POINT('Ctrl Pts',(11.6778970386953,1.39579479040469,0.605695249702978));
#13423=CARTESIAN_POINT('Ctrl Pts',(11.7375219088137,1.42469609383707,-0.000371738767665111));
#13424=CARTESIAN_POINT('Ctrl Pts',(11.7269244310859,1.41412622652679,0.202087962343291));
#13425=CARTESIAN_POINT('Ctrl Pts',(11.7163270893473,1.40355692684423,0.404547700208143));
#13426=CARTESIAN_POINT('Ctrl Pts',(11.7057297418778,1.39298745758592,0.607007427831054));
#13427=CARTESIAN_POINT('Ctrl Pts',(11.7837126264455,1.39812338730171,0.000662527065309348));
#13428=CARTESIAN_POINT('Ctrl Pts',(11.7731059659782,1.38755170250994,0.203121672627585));
#13429=CARTESIAN_POINT('Ctrl Pts',(11.762499302106,1.37698011891703,0.405580822779681));
#13430=CARTESIAN_POINT('Ctrl Pts',(11.7518926781287,1.36640881816393,0.608039989525598));
#13431=CARTESIAN_POINT('Ctrl Pts',(11.7997807104374,1.34910745421534,-0.00105289019631603));
#13432=CARTESIAN_POINT('Ctrl Pts',(11.7891702365097,1.33854134055748,0.201406383632416));
#13433=CARTESIAN_POINT('Ctrl Pts',(11.7785598611315,1.32797539467558,0.403865671186622));
#13434=CARTESIAN_POINT('Ctrl Pts',(11.7679493857164,1.31740972279341,0.60632496775791));
#13435=CARTESIAN_POINT('Ctrl Pts',(11.7998379289556,1.32812520727701,-0.00214468456243374));
#13436=CARTESIAN_POINT('Ctrl Pts',(11.78922748064,1.31756145959839,0.200314730064766));
#13437=CARTESIAN_POINT('Ctrl Pts',(11.7786170316934,1.30699794333589,0.402774156733522));
#13438=CARTESIAN_POINT('Ctrl Pts',(11.7680065821063,1.2964346619681,0.605233595624295));
#13439=CARTESIAN_POINT('Ctrl Pts',(11.7680065821063,1.2964346619681,0.605233595624295));
#13440=CARTESIAN_POINT('Ctrl Pts',(11.7785795656372,1.30696064383315,0.403489051673192));
#13441=CARTESIAN_POINT('Ctrl Pts',(11.7891525485321,1.31748685893698,0.201744519857946));
#13442=CARTESIAN_POINT('Ctrl Pts',(11.7997255308004,1.32801330383774,3.10081821330854E-17));
#13443=CARTESIAN_POINT('Ctrl Pts',(11.3905090053564,1.32332268868375,0.7));
#13444=CARTESIAN_POINT('Ctrl Pts',(11.4830653488871,1.31448403714216,0.7));
#13445=CARTESIAN_POINT('Ctrl Pts',(11.5756099286391,1.3055179747114,0.7));
#13446=CARTESIAN_POINT('Ctrl Pts',(11.6681436286308,1.2964346619681,0.7));
#13447=CARTESIAN_POINT('Ctrl Pts',(11.3932507170007,1.35203326785047,0.7));
#13448=CARTESIAN_POINT('Ctrl Pts',(11.4858332859074,1.34318985044544,0.699999917777441));
#13449=CARTESIAN_POINT('Ctrl Pts',(11.5784027531871,1.33421922733773,0.700000082825348));
#13450=CARTESIAN_POINT('Ctrl Pts',(11.6709605510772,1.32513126902304,0.7));
#13451=CARTESIAN_POINT('Ctrl Pts',(11.3980029235658,1.40179729139028,0.67675176769038));
#13452=CARTESIAN_POINT('Ctrl Pts',(11.4906306781252,1.39294591144353,0.676755553516685));
#13453=CARTESIAN_POINT('Ctrl Pts',(11.583243842395,1.38396722707511,0.676759299309383));
#13454=CARTESIAN_POINT('Ctrl Pts',(11.6758431636759,1.37487151491717,0.676763114282959));
#13455=CARTESIAN_POINT('Ctrl Pts',(11.3998836071583,1.4214913811319,0.627256563056779));
#13456=CARTESIAN_POINT('Ctrl Pts',(11.4925297866457,1.41264104586547,0.627266369072496));
#13457=CARTESIAN_POINT('Ctrl Pts',(11.5851604051362,1.40366358810601,0.627276165220861));
#13458=CARTESIAN_POINT('Ctrl Pts',(11.6777767156198,1.39456903283364,0.627286048421068));
#13459=CARTESIAN_POINT('Ctrl Pts',(11.4,1.4227102204299,0.605660349289938));
#13460=CARTESIAN_POINT('Ctrl Pts',(11.4926474653491,1.41386220753305,0.605671932550561));
#13461=CARTESIAN_POINT('Ctrl Pts',(11.585279512325,1.40488700096013,0.605683574233495));
#13462=CARTESIAN_POINT('Ctrl Pts',(11.6778970386953,1.39579479040469,0.605695249702977));
#13463=CARTESIAN_POINT('Ctrl Pts',(0.200160078391861,1.15273809776858,-0.00218270663797729));
#13464=CARTESIAN_POINT('Ctrl Pts',(0.210771190526905,1.14220881798213,0.200289374419605));
#13465=CARTESIAN_POINT('Ctrl Pts',(0.221382303689445,1.13167991623912,0.402761475082968));
#13466=CARTESIAN_POINT('Ctrl Pts',(0.231993417893744,1.12115139781563,0.605233595624295));
#13467=CARTESIAN_POINT('Ctrl Pts',(0.200222527243758,1.17571472979894,-0.000991111558954063));
#13468=CARTESIAN_POINT('Ctrl Pts',(0.210833737189325,1.165180254798,0.201480665494204));
#13469=CARTESIAN_POINT('Ctrl Pts',(0.22144460713556,1.15464621893915,0.403952483115279));
#13470=CARTESIAN_POINT('Ctrl Pts',(0.232055819885544,1.1441124535127,0.606424296559433));
#13471=CARTESIAN_POINT('Ctrl Pts',(0.216855804290742,1.22156704800519,0.000521661548984882));
#13472=CARTESIAN_POINT('Ctrl Pts',(0.22745908713481,1.21102245544698,0.202993270772045));
#13473=CARTESIAN_POINT('Ctrl Pts',(0.238062502254218,1.2004779673848,0.405464877727456));
#13474=CARTESIAN_POINT('Ctrl Pts',(0.248665715176951,1.18993398276804,0.607936521147589));
#13475=CARTESIAN_POINT('Ctrl Pts',(0.258823218619159,1.24645290953083,-0.000383602721372307));
#13476=CARTESIAN_POINT('Ctrl Pts',(0.269410282911183,1.23591162135389,0.202088997034388));
#13477=CARTESIAN_POINT('Ctrl Pts',(0.279997195000074,1.22537100634993,0.404561639451295));
#13478=CARTESIAN_POINT('Ctrl Pts',(0.290584031570127,1.21483034200885,0.60703428203898));
#13479=CARTESIAN_POINT('Ctrl Pts',(0.281396145950812,1.25079993650842,-0.00134053860524368));
#13480=CARTESIAN_POINT('Ctrl Pts',(0.291976789318506,1.24026479669674,0.201132712115111));
#13481=CARTESIAN_POINT('Ctrl Pts',(0.302557285401186,1.22972999171968,0.403605987142707));
#13482=CARTESIAN_POINT('Ctrl Pts',(0.313137632044028,1.21919552599286,0.606079286803922));
#13483=CARTESIAN_POINT('Origin',(11.8002740930491,1.6,-0.0104671912485888));
#13484=CARTESIAN_POINT('Origin',(0.3318563713692,1.12115139781563,0.6));
#13485=CARTESIAN_POINT('',(0.331856371369203,1.12115139781563,0.9));
#13486=CARTESIAN_POINT('',(0.0322675109428288,1.12115139781563,0.615700786872883));
#13487=CARTESIAN_POINT('Origin',(0.3318563713692,1.12115139781563,0.6));
#13488=CARTESIAN_POINT('',(0.275700153393682,1.4152837823473,0.618237860411764));
#13489=CARTESIAN_POINT('Origin',(0.3318563713692,1.12115139781563,0.6));
#13490=CARTESIAN_POINT('Origin',(0.331856371369201,1.12115139781563,0.600000000000001));
#13491=CARTESIAN_POINT('Origin',(11.6681436286308,1.2964346619681,0.6));
#13492=CARTESIAN_POINT('',(11.6681436286308,1.2964346619681,0.9));
#13493=CARTESIAN_POINT('',(11.6974038588243,1.59451504727786,0.617085749108931));
#13494=CARTESIAN_POINT('Origin',(11.6681436286308,1.2964346619681,0.6));
#13495=CARTESIAN_POINT('',(11.9677324890572,1.2964346619681,0.615700786872884));
#13496=CARTESIAN_POINT('Origin',(11.6681436286308,1.2964346619681,0.6));
#13497=CARTESIAN_POINT('Origin',(11.6681436286308,1.2964346619681,0.6));
#13498=CARTESIAN_POINT('Origin',(0.3318563713692,-1.12115139781563,0.6));
#13499=CARTESIAN_POINT('',(0.3318563713692,-1.12115139781563,0.9));
#13500=CARTESIAN_POINT('',(0.27570015339368,-1.4152837823473,0.618237860411764));
#13501=CARTESIAN_POINT('Origin',(0.331856371369206,-1.12115139781563,0.6));
#13502=CARTESIAN_POINT('',(0.0322675109428289,-1.12115139781563,0.615700786872884));
#13503=CARTESIAN_POINT('Origin',(0.3318563713692,-1.12115139781563,0.6));
#13504=CARTESIAN_POINT('Origin',(0.331856371369201,-1.12115139781563,0.6));
#13505=CARTESIAN_POINT('Origin',(0.3318563713692,-0.7,0.6));
#13506=CARTESIAN_POINT('',(0.0322675109428288,-0.7,0.615700786872883));
#13507=CARTESIAN_POINT('',(0.3318563713692,-0.7,0.9));
#13508=CARTESIAN_POINT('Ctrl Pts',(0.243379792658812,-1.44768816351885,
-0.00386660544379547));
#13509=CARTESIAN_POINT('Ctrl Pts',(0.254153714020244,-1.43688644166428,
0.203501514337738));
#13510=CARTESIAN_POINT('Ctrl Pts',(0.264927169923045,-1.42608498030896,
0.410869669467268));
#13511=CARTESIAN_POINT('Ctrl Pts',(0.275700153393682,-1.4152837823473,0.618237860411764));
#13512=CARTESIAN_POINT('Ctrl Pts',(0.165985306518657,-1.43278556900406,
-0.000585522405354874));
#13513=CARTESIAN_POINT('Ctrl Pts',(0.176781886982148,-1.42196211044871,
0.206780297826791));
#13514=CARTESIAN_POINT('Ctrl Pts',(0.187577631459021,-1.41114055376332,
0.414146260476818));
#13515=CARTESIAN_POINT('Ctrl Pts',(0.198373523197449,-1.40031743725927,
0.621512129789107));
#13516=CARTESIAN_POINT('Ctrl Pts',(0.0420337764471552,-1.35067831466576,
0.00164062070145552));
#13517=CARTESIAN_POINT('Ctrl Pts',(0.0528811856485653,-1.33984924001505,
0.209003590924217));
#13518=CARTESIAN_POINT('Ctrl Pts',(0.0637288270387668,-1.3290196870647,
0.416366521726085));
#13519=CARTESIAN_POINT('Ctrl Pts',(0.0745760486629849,-1.31819094697801,
0.623729515932473));
#13520=CARTESIAN_POINT('Ctrl Pts',(-0.000174449685670057,-1.21258510413485,
-0.00332869829739982));
#13521=CARTESIAN_POINT('Ctrl Pts',(0.0106931634330696,-1.20178787588112,
0.204035045544629));
#13522=CARTESIAN_POINT('Ctrl Pts',(0.0215603573327632,-1.19099068058357,
0.411398812224037));
#13523=CARTESIAN_POINT('Ctrl Pts',(0.0324279732074593,-1.18019411246525,
0.618762589277523));
#13524=CARTESIAN_POINT('Ctrl Pts',(-0.000335035344191381,-1.15350137313465,
-0.00639285519773308));
#13525=CARTESIAN_POINT('Ctrl Pts',(0.0105324790023165,-1.1427176497384,
0.200971671503832));
#13526=CARTESIAN_POINT('Ctrl Pts',(0.0213999944262164,-1.13193432274319,
0.408336218763261));
#13527=CARTESIAN_POINT('Ctrl Pts',(0.0322675109428286,-1.12115139781563,
0.615700786872884));
#13528=CARTESIAN_POINT('Ctrl Pts',(0.243580684154575,-1.44748675362873,
-2.16840434497101E-17));
#13529=CARTESIAN_POINT('Ctrl Pts',(0.254287635915809,-1.43675217163244,
0.206079251738322));
#13530=CARTESIAN_POINT('Ctrl Pts',(0.264994127943615,-1.42601784692504,
0.412158538389471));
#13531=CARTESIAN_POINT('Ctrl Pts',(0.275700153393682,-1.4152837823473,0.618237860411764));
#13532=CARTESIAN_POINT('Ctrl Pts',(0.0322675109428286,-1.12115139781563,
0.615700786872884));
#13533=CARTESIAN_POINT('Ctrl Pts',(0.0215116728964671,-1.13182351356624,
0.410467170919192));
#13534=CARTESIAN_POINT('Ctrl Pts',(0.0107558359204751,-1.14249602316337,
0.205233575389367));
#13535=CARTESIAN_POINT('Ctrl Pts',(-1.41190227911925E-16,-1.15316892111333,
8.06646416329215E-17));
#13536=CARTESIAN_POINT('Origin',(11.6681436286308,-1.2964346619681,0.6));
#13537=CARTESIAN_POINT('',(11.9677324890572,-1.2964346619681,0.615700786872884));
#13538=CARTESIAN_POINT('',(11.6974038588243,-1.59451504727786,0.617085749108931));
#13539=CARTESIAN_POINT('Origin',(11.6681436286308,-1.2964346619681,0.600000000000001));
#13540=CARTESIAN_POINT('',(11.6681436286308,-1.2964346619681,0.9));
#13541=CARTESIAN_POINT('Origin',(11.6681436286308,-1.2964346619681,0.6));
#13542=CARTESIAN_POINT('Origin',(11.6681436286308,-1.2964346619681,0.6));
#13543=CARTESIAN_POINT('Origin',(11.6681436286308,0.8,0.6));
#13544=CARTESIAN_POINT('',(11.9677324890572,0.8,0.615700786872884));
#13545=CARTESIAN_POINT('',(11.6681436286308,0.8,0.9));
#13546=CARTESIAN_POINT('Ctrl Pts',(11.6681436286308,-1.2964346619681,0.9));
#13547=CARTESIAN_POINT('Ctrl Pts',(10.0505146497799,-1.45522470190849,0.9));
#13548=CARTESIAN_POINT('Ctrl Pts',(7.34698379851713,-1.66064017564263,0.9));
#13549=CARTESIAN_POINT('Ctrl Pts',(3.5507249968367,-1.5921338472202,0.9));
#13550=CARTESIAN_POINT('Ctrl Pts',(1.39628032950236,-1.32437289587156,0.9));
#13551=CARTESIAN_POINT('Ctrl Pts',(0.331856371369199,-1.12115139781563,
0.9));
#13552=CARTESIAN_POINT('Ctrl Pts',(11.6765943959699,-1.38252448313292,0.9));
#13553=CARTESIAN_POINT('Ctrl Pts',(10.0577014803155,-1.54155822929668,0.900004386952174));
#13554=CARTESIAN_POINT('Ctrl Pts',(7.35045927226653,-1.74750661992774,0.90000020513805));
#13555=CARTESIAN_POINT('Ctrl Pts',(3.54497585078588,-1.67885197560093,0.899998846478116));
#13556=CARTESIAN_POINT('Ctrl Pts',(1.38372480803625,-1.41002339692611,0.900007381454799));
#13557=CARTESIAN_POINT('Ctrl Pts',(0.315675209020016,-1.2059043252356,0.9));
#13558=CARTESIAN_POINT('Ctrl Pts',(11.6912432102654,-1.53175516862908,0.830242007927396));
#13559=CARTESIAN_POINT('Ctrl Pts',(10.070172518288,-1.69119563674726,0.830042231904815));
#13560=CARTESIAN_POINT('Ctrl Pts',(7.35645297288469,-1.89806162871739,0.829725685238203));
#13561=CARTESIAN_POINT('Ctrl Pts',(3.53503777381493,-1.8291593714544,0.829829026055289));
#13562=CARTESIAN_POINT('Ctrl Pts',(1.36192166831068,-1.55847530615989,0.830279056498203));
#13563=CARTESIAN_POINT('Ctrl Pts',(0.28762358730286,-1.35283178372728,0.830616544072481));
#13564=CARTESIAN_POINT('Ctrl Pts',(11.6970428895979,-1.59083777456472,0.681858145263203));
#13565=CARTESIAN_POINT('Ctrl Pts',(10.0750816081461,-1.75021732245097,0.681339641080976));
#13566=CARTESIAN_POINT('Ctrl Pts',(7.3588078744758,-1.95708146899443,0.680519979048775));
#13567=CARTESIAN_POINT('Ctrl Pts',(3.53113644431293,-1.88819699008302,0.68078748362792));
#13568=CARTESIAN_POINT('Ctrl Pts',(1.35331700817769,-1.61730376958615,0.681953432622034));
#13569=CARTESIAN_POINT('Ctrl Pts',(0.276437927844241,-1.41141950219787,
0.682830994206899));
#13570=CARTESIAN_POINT('Ctrl Pts',(11.6974038588243,-1.59451504727786,0.617085749108931));
#13571=CARTESIAN_POINT('Ctrl Pts',(10.0753786444688,-1.75377172884558,0.616473434532366));
#13572=CARTESIAN_POINT('Ctrl Pts',(7.35893161235257,-1.96044797105896,0.61550283428964));
#13573=CARTESIAN_POINT('Ctrl Pts',(3.53092277948893,-1.89162724517065,0.615818637525046));
#13574=CARTESIAN_POINT('Ctrl Pts',(1.35277799022997,-1.62098550016515,0.617200513836093));
#13575=CARTESIAN_POINT('Ctrl Pts',(0.27570015339368,-1.4152837823473,0.618237860411764));
#13576=CARTESIAN_POINT('Ctrl Pts',(0.27570015339368,-1.4152837823473,0.618237860411764));
#13577=CARTESIAN_POINT('Ctrl Pts',(1.35277799022997,-1.62098550016515,0.617200513836093));
#13578=CARTESIAN_POINT('Ctrl Pts',(3.53092277948893,-1.89162724517065,0.615818637525046));
#13579=CARTESIAN_POINT('Ctrl Pts',(7.35893161235257,-1.96044797105896,0.61550283428964));
#13580=CARTESIAN_POINT('Ctrl Pts',(10.0753786444688,-1.75377172884558,0.616473434532366));
#13581=CARTESIAN_POINT('Ctrl Pts',(11.6974038588243,-1.59451504727786,0.617085749108931));
#13582=CARTESIAN_POINT('Ctrl Pts',(11.6681436286308,-1.2964346619681,0.9));
#13583=CARTESIAN_POINT('Ctrl Pts',(10.0505146497799,-1.45522470190849,0.9));
#13584=CARTESIAN_POINT('Ctrl Pts',(7.34698379851713,-1.66064017564263,0.9));
#13585=CARTESIAN_POINT('Ctrl Pts',(3.5507249968367,-1.5921338472202,0.9));
#13586=CARTESIAN_POINT('Ctrl Pts',(1.39628032950236,-1.32437289587156,0.9));
#13587=CARTESIAN_POINT('Ctrl Pts',(0.331856371369199,-1.12115139781563,
0.9));
#13588=CARTESIAN_POINT('Ctrl Pts',(12.0003454972153,-1.32890342861544,-0.00659247958978532));
#13589=CARTESIAN_POINT('Ctrl Pts',(11.9894744951615,-1.31808026232082,0.200838596530835));
#13590=CARTESIAN_POINT('Ctrl Pts',(11.9786034924455,-1.30725733885828,0.408269685287046));
#13591=CARTESIAN_POINT('Ctrl Pts',(11.9677324890572,-1.2964346619681,0.615700786872884));
#13592=CARTESIAN_POINT('Ctrl Pts',(12.000116620981,-1.41283311850955,-0.00222526087931226));
#13593=CARTESIAN_POINT('Ctrl Pts',(11.9892453109784,-1.40200002127642,0.205205215027088));
#13594=CARTESIAN_POINT('Ctrl Pts',(11.9783750177566,-1.39116761830557,0.412635780645844));
#13595=CARTESIAN_POINT('Ctrl Pts',(11.9675037034976,-1.38033490526933,0.620066275407343));
#13596=CARTESIAN_POINT('Ctrl Pts',(11.9341774721098,-1.5584705948029,0.00191796595980313));
#13597=CARTESIAN_POINT('Ctrl Pts',(11.9233226835938,-1.54762133657986,0.209348350794306));
#13598=CARTESIAN_POINT('Ctrl Pts',(11.9124678718222,-1.53677206634062,0.416778732304926));
#13599=CARTESIAN_POINT('Ctrl Pts',(11.9016132473252,-1.52592301942363,0.624209134118803));
#13600=CARTESIAN_POINT('Ctrl Pts',(11.7925116537096,-1.62071287545028,-0.0022587989925734));
#13601=CARTESIAN_POINT('Ctrl Pts',(11.7816834491585,-1.6098745265243,0.205173499361722));
#13602=CARTESIAN_POINT('Ctrl Pts',(11.7708551999607,-1.59903658749835,0.41260581547062));
#13603=CARTESIAN_POINT('Ctrl Pts',(11.760027440985,-1.58819854843564,0.620038149897102));
#13604=CARTESIAN_POINT('Ctrl Pts',(11.7298629188572,-1.62699926142283,-0.0052140742384003));
#13605=CARTESIAN_POINT('Ctrl Pts',(11.7190429637906,-1.61617098622686,0.202219177289036));
#13606=CARTESIAN_POINT('Ctrl Pts',(11.708223275703,-1.60534291388117,0.409652451626141));
#13607=CARTESIAN_POINT('Ctrl Pts',(11.6974038588243,-1.59451504727786,0.617085749108931));
#13608=CARTESIAN_POINT('Ctrl Pts',(12.,-1.32855945177638,-1.94722710178397E-16));
#13609=CARTESIAN_POINT('Ctrl Pts',(11.9892441636707,-1.31785094954632,0.205233583190348));
#13610=CARTESIAN_POINT('Ctrl Pts',(11.978488326693,-1.30714268506935,0.410467178751997));
#13611=CARTESIAN_POINT('Ctrl Pts',(11.9677324890572,-1.2964346619681,0.615700786872884));
#13612=CARTESIAN_POINT('Ctrl Pts',(11.6974038588243,-1.59451504727786,0.617085749108931));
#13613=CARTESIAN_POINT('Ctrl Pts',(11.7081326228587,-1.605252190239,0.41139047675572));
#13614=CARTESIAN_POINT('Ctrl Pts',(11.7188616535763,-1.61598953550924,0.205695227161956));
#13615=CARTESIAN_POINT('Ctrl Pts',(11.7295909468525,-1.62672708026858,8.73866951023317E-17));
#13616=CARTESIAN_POINT('Ctrl Pts',(11.7298546566854,1.62699099289774,-0.00505567716946009));
#13617=CARTESIAN_POINT('Ctrl Pts',(11.719037455812,1.61616547398006,0.202324775346606));
#13618=CARTESIAN_POINT('Ctrl Pts',(11.7082205217827,1.60534015781013,0.409705250660816));
#13619=CARTESIAN_POINT('Ctrl Pts',(11.6974038588243,1.59451504727786,0.617085749108931));
#13620=CARTESIAN_POINT('Ctrl Pts',(11.8133862946664,1.61860913476435,-0.00111531114554236));
#13621=CARTESIAN_POINT('Ctrl Pts',(11.8025579038448,1.6077699189899,0.206263846261978));
#13622=CARTESIAN_POINT('Ctrl Pts',(11.7917299466398,1.59693199028804,0.41364309356145));
#13623=CARTESIAN_POINT('Ctrl Pts',(11.7809019683719,1.58609304882157,0.621022283493159));
#13624=CARTESIAN_POINT('Ctrl Pts',(11.9519653779615,1.53884931758497,0.00198566945999789));
#13625=CARTESIAN_POINT('Ctrl Pts',(11.9411087765487,1.52800449744246,0.209363119024413));
#13626=CARTESIAN_POINT('Ctrl Pts',(11.9302521502216,1.51715965702667,0.416740564833343));
#13627=CARTESIAN_POINT('Ctrl Pts',(11.9193956662674,1.50631506689811,0.624118030142866));
#13628=CARTESIAN_POINT('Ctrl Pts',(12.0001655389052,1.39184242582033,-0.00315867047762133));
#13629=CARTESIAN_POINT('Ctrl Pts',(11.9892972278067,1.38101476165208,0.204219175612729));
#13630=CARTESIAN_POINT('Ctrl Pts',(11.9784292129672,1.37018709651964,0.41159703650799));
#13631=CARTESIAN_POINT('Ctrl Pts',(11.9675608998875,1.35935984444403,0.618974903273729));
#13632=CARTESIAN_POINT('Ctrl Pts',(12.0003371960637,1.32889516399154,-0.00643408418199817));
#13633=CARTESIAN_POINT('Ctrl Pts',(11.9894689610601,1.31807475269516,0.200944193475792));
#13634=CARTESIAN_POINT('Ctrl Pts',(11.9786007253947,1.3072545841082,0.408322483762789));
#13635=CARTESIAN_POINT('Ctrl Pts',(11.9677324890572,1.2964346619681,0.615700786872884));
#13636=CARTESIAN_POINT('Ctrl Pts',(11.7295909468525,1.62672708026857,-8.50014503228635E-17));
#13637=CARTESIAN_POINT('Ctrl Pts',(11.7188616535763,1.61598953550924,0.205695227161956));
#13638=CARTESIAN_POINT('Ctrl Pts',(11.7081326228587,1.605252190239,0.411390476755719));
#13639=CARTESIAN_POINT('Ctrl Pts',(11.6974038588243,1.59451504727786,0.617085749108931));
#13640=CARTESIAN_POINT('Ctrl Pts',(11.9677324890572,1.2964346619681,0.615700786872884));
#13641=CARTESIAN_POINT('Ctrl Pts',(11.978488326693,1.30714268506935,0.410467178751997));
#13642=CARTESIAN_POINT('Ctrl Pts',(11.9892441636707,1.31785094954633,0.205233583190349));
#13643=CARTESIAN_POINT('Ctrl Pts',(12.,1.32855945177638,-2.38524477946811E-17));
#13644=CARTESIAN_POINT('Ctrl Pts',(0.3318563713692,1.12115139781563,0.9));
#13645=CARTESIAN_POINT('Ctrl Pts',(1.92849230856897,1.42598364489954,0.9));
#13646=CARTESIAN_POINT('Ctrl Pts',(5.71993880054687,1.76935652211139,0.9));
#13647=CARTESIAN_POINT('Ctrl Pts',(9.51130499016288,1.50815471522196,0.9));
#13648=CARTESIAN_POINT('Ctrl Pts',(11.6681436286308,1.2964346619681,0.9));
#13649=CARTESIAN_POINT('Ctrl Pts',(0.315675209020018,1.2059043252356,0.9));
#13650=CARTESIAN_POINT('Ctrl Pts',(1.91774960754439,1.51208293277137,0.900011072182198));
#13651=CARTESIAN_POINT('Ctrl Pts',(5.72069615836457,1.85663493780214,0.899990666655967));
#13652=CARTESIAN_POINT('Ctrl Pts',(9.5180705084307,1.59456947801794,0.900005849269565));
#13653=CARTESIAN_POINT('Ctrl Pts',(11.6765943959699,1.38252448313292,0.9));
#13654=CARTESIAN_POINT('Ctrl Pts',(0.287623587302861,1.35283178372728,0.83061654407248));
#13655=CARTESIAN_POINT('Ctrl Pts',(1.89907070881462,1.6612970673762,0.830110312711064));
#13656=CARTESIAN_POINT('Ctrl Pts',(5.72203120258494,2.00791989451774,0.829536565111056));
#13657=CARTESIAN_POINT('Ctrl Pts',(9.52981562096212,1.74434245945332,0.829975639897288));
#13658=CARTESIAN_POINT('Ctrl Pts',(11.6912432102654,1.53175516862908,0.830242007927395));
#13659=CARTESIAN_POINT('Ctrl Pts',(0.276437927844243,1.41141950219787,0.682830994206899));
#13660=CARTESIAN_POINT('Ctrl Pts',(1.89175654834445,1.7202459032803,0.681514651829601));
#13661=CARTESIAN_POINT('Ctrl Pts',(5.72254254462207,2.06699613896002,0.680031275065471));
#13662=CARTESIAN_POINT('Ctrl Pts',(9.53442784766217,1.80334383841306,0.681166806353567));
#13663=CARTESIAN_POINT('Ctrl Pts',(11.6970428895979,1.59083777456472,0.681858145263204));
#13664=CARTESIAN_POINT('Ctrl Pts',(0.275700153393682,1.4152837823473,0.618237860411764));
#13665=CARTESIAN_POINT('Ctrl Pts',(1.89131690864814,1.72383635907408,0.616681840548257));
#13666=CARTESIAN_POINT('Ctrl Pts',(5.72257555688819,2.07025489722917,0.614922376024419));
#13667=CARTESIAN_POINT('Ctrl Pts',(9.53470357301702,1.80685728936816,0.616269329673511));
#13668=CARTESIAN_POINT('Ctrl Pts',(11.6974038588243,1.59451504727786,0.617085749108931));
#13669=CARTESIAN_POINT('Ctrl Pts',(11.6974038588243,1.59451504727786,0.617085749108931));
#13670=CARTESIAN_POINT('Ctrl Pts',(9.53470357301702,1.80685728936816,0.616269329673511));
#13671=CARTESIAN_POINT('Ctrl Pts',(5.72257555688819,2.07025489722917,0.614922376024419));
#13672=CARTESIAN_POINT('Ctrl Pts',(1.89131690864814,1.72383635907408,0.616681840548257));
#13673=CARTESIAN_POINT('Ctrl Pts',(0.275700153393682,1.4152837823473,0.618237860411764));
#13674=CARTESIAN_POINT('Ctrl Pts',(0.3318563713692,1.12115139781563,0.9));
#13675=CARTESIAN_POINT('Ctrl Pts',(1.92849230856897,1.42598364489954,0.9));
#13676=CARTESIAN_POINT('Ctrl Pts',(5.71993880054687,1.76935652211139,0.9));
#13677=CARTESIAN_POINT('Ctrl Pts',(9.51130499016288,1.50815471522196,0.9));
#13678=CARTESIAN_POINT('Ctrl Pts',(11.6681436286308,1.2964346619681,0.9));
#13679=CARTESIAN_POINT('Ctrl Pts',(-0.000343174493958709,1.15350944952984,
-0.00654815942696785));
#13680=CARTESIAN_POINT('Ctrl Pts',(0.0105270529019337,1.14272303380391,
0.200868135340743));
#13681=CARTESIAN_POINT('Ctrl Pts',(0.0213972813757523,1.13193701467556,
0.408284450676511));
#13682=CARTESIAN_POINT('Ctrl Pts',(0.0322675109428289,1.12115139781563,
0.615700786872884));
#13683=CARTESIAN_POINT('Ctrl Pts',(-0.000129060241737355,1.23228777111366,
-0.0024626161135415));
#13684=CARTESIAN_POINT('Ctrl Pts',(0.0107416412387167,1.22148297235423,
0.204952596860618));
#13685=CARTESIAN_POINT('Ctrl Pts',(0.0216107531875107,1.21067920461451,
0.412367946918899));
#13686=CARTESIAN_POINT('Ctrl Pts',(0.0324814606290031,1.19987501734845,
0.61978319007907));
#13687=CARTESIAN_POINT('Ctrl Pts',(0.0574602827844584,1.36931747586956,
0.00164530659801973));
#13688=CARTESIAN_POINT('Ctrl Pts',(0.0683025556324749,1.35848226928888,
0.209060253413207));
#13689=CARTESIAN_POINT('Ctrl Pts',(0.079145272670006,1.34764679267913,0.416475160658282));
#13690=CARTESIAN_POINT('Ctrl Pts',(0.0899872847341513,1.33681188280878,
0.62389013300849));
#13691=CARTESIAN_POINT('Ctrl Pts',(0.185325846363896,1.43651931939441,-0.00156109881554352));
#13692=CARTESIAN_POINT('Ctrl Pts',(0.196119220517603,1.4256988926218,0.205857093047737));
#13693=CARTESIAN_POINT('Ctrl Pts',(0.20691256009293,1.41487906031557,0.413275315721495));
#13694=CARTESIAN_POINT('Ctrl Pts',(0.217705180746507,1.40405902353128,0.620693562444772));
#13695=CARTESIAN_POINT('Ctrl Pts',(0.243371723604776,1.44769625339383,-0.00402191236404));
#13696=CARTESIAN_POINT('Ctrl Pts',(0.254148334883323,1.43689183478419,0.203397976373256));
#13697=CARTESIAN_POINT('Ctrl Pts',(0.264924480472538,1.42608767680315,0.410817900476086));
#13698=CARTESIAN_POINT('Ctrl Pts',(0.275700153393682,1.4152837823473,0.618237860411764));
#13699=CARTESIAN_POINT('Ctrl Pts',(-1.23734572934908E-17,1.15316892111333,
-8.67361737988404E-19));
#13700=CARTESIAN_POINT('Ctrl Pts',(0.0107558359204753,1.14249602316336,
0.205233575389367));
#13701=CARTESIAN_POINT('Ctrl Pts',(0.0215116728964674,1.13182351356624,
0.410467170919192));
#13702=CARTESIAN_POINT('Ctrl Pts',(0.0322675109428289,1.12115139781563,
0.615700786872884));
#13703=CARTESIAN_POINT('Ctrl Pts',(0.275700153393682,1.4152837823473,0.618237860411764));
#13704=CARTESIAN_POINT('Ctrl Pts',(0.264994127943615,1.42601784692504,0.412158538389472));
#13705=CARTESIAN_POINT('Ctrl Pts',(0.254287635915814,1.43675217163244,0.206079251738322));
#13706=CARTESIAN_POINT('Ctrl Pts',(0.243580684154575,1.44748675362873,-1.9298798670242E-17));
#13707=CARTESIAN_POINT('Ctrl Pts',(11.7295909468525,-1.62672708026858,0.));
#13708=CARTESIAN_POINT('Ctrl Pts',(11.7192775324813,-1.61592692249094,0.206079286804135));
#13709=CARTESIAN_POINT('Ctrl Pts',(11.70896411811,-1.6051267647133,0.41215857360827));
#13710=CARTESIAN_POINT('Ctrl Pts',(11.6986507037388,-1.59432660693566,0.618237860412405));
#13711=CARTESIAN_POINT('Ctrl Pts',(7.90092085928651,-2.00057770191527,0.));
#13712=CARTESIAN_POINT('Ctrl Pts',(7.89749915175266,-1.98977754413763,0.206079286804135));
#13713=CARTESIAN_POINT('Ctrl Pts',(7.89407744421881,-1.97897738636,0.41215857360827));
#13714=CARTESIAN_POINT('Ctrl Pts',(7.89065573668496,-1.96817722858236,0.618237860412405));
#13715=CARTESIAN_POINT('Ctrl Pts',(4.07225077172054,-2.17467835246083,0.));
#13716=CARTESIAN_POINT('Ctrl Pts',(4.07572077102407,-2.16387819468319,0.206079286804135));
#13717=CARTESIAN_POINT('Ctrl Pts',(4.07919077032759,-2.15307803690555,0.41215857360827));
#13718=CARTESIAN_POINT('Ctrl Pts',(4.08266076963111,-2.14227787912792,0.618237860412405));
#13719=CARTESIAN_POINT('Ctrl Pts',(0.243580684154574,-1.44748675362873,
0.));
#13720=CARTESIAN_POINT('Ctrl Pts',(0.253942390295469,-1.43668659585109,
0.206079286804135));
#13721=CARTESIAN_POINT('Ctrl Pts',(0.264304096436365,-1.42588643807345,
0.41215857360827));
#13722=CARTESIAN_POINT('Ctrl Pts',(0.27466580257726,-1.41508628029581,0.618237860412405));
#13723=CARTESIAN_POINT('Origin',(0.,-1.4,0.));
#13724=CARTESIAN_POINT('Origin',(6.08012166120517,1.06803409199199E-16,
0.9));
#13725=CARTESIAN_POINT('Ctrl Pts',(0.243580684154574,1.44748675362873,0.));
#13726=CARTESIAN_POINT('Ctrl Pts',(0.253942390295469,1.43668659585109,0.206079286804135));
#13727=CARTESIAN_POINT('Ctrl Pts',(0.264304096436365,1.42588643807345,0.41215857360827));
#13728=CARTESIAN_POINT('Ctrl Pts',(0.27466580257726,1.41508628029581,0.618237860412405));
#13729=CARTESIAN_POINT('Ctrl Pts',(4.07225077172054,2.17467835246083,0.));
#13730=CARTESIAN_POINT('Ctrl Pts',(4.07572077102407,2.16387819468319,0.206079286804135));
#13731=CARTESIAN_POINT('Ctrl Pts',(4.07919077032759,2.15307803690555,0.41215857360827));
#13732=CARTESIAN_POINT('Ctrl Pts',(4.08266076963111,2.14227787912792,0.618237860412405));
#13733=CARTESIAN_POINT('Ctrl Pts',(7.90092085928651,2.00057770191527,0.));
#13734=CARTESIAN_POINT('Ctrl Pts',(7.89749915175266,1.98977754413763,0.206079286804135));
#13735=CARTESIAN_POINT('Ctrl Pts',(7.89407744421881,1.97897738636,0.41215857360827));
#13736=CARTESIAN_POINT('Ctrl Pts',(7.89065573668496,1.96817722858236,0.618237860412405));
#13737=CARTESIAN_POINT('Ctrl Pts',(11.7295909468525,1.62672708026858,0.));
#13738=CARTESIAN_POINT('Ctrl Pts',(11.7192775324813,1.61592692249094,0.206079286804135));
#13739=CARTESIAN_POINT('Ctrl Pts',(11.70896411811,1.6051267647133,0.41215857360827));
#13740=CARTESIAN_POINT('Ctrl Pts',(11.6986507037388,1.59432660693566,0.618237860412405));
#13741=CARTESIAN_POINT('Origin',(12.,1.6,0.));
#13742=CARTESIAN_POINT('',(0.,0.,0.));
#13743=CARTESIAN_POINT('Origin',(2.,0.,1.));
#13744=CARTESIAN_POINT('',(1.65,4.28626379701574E-17,1.1));
#13745=CARTESIAN_POINT('Origin',(2.,0.,1.1));
#13746=CARTESIAN_POINT('',(1.65,4.28626379701574E-17,0.9));
#13747=CARTESIAN_POINT('',(1.65,4.28626379701574E-17,1.));
#13748=CARTESIAN_POINT('Origin',(2.,0.,0.9));
#13749=CARTESIAN_POINT('Origin',(10.,0.,1.));
#13750=CARTESIAN_POINT('',(9.65,4.28626379701574E-17,1.1));
#13751=CARTESIAN_POINT('Origin',(10.,0.,1.1));
#13752=CARTESIAN_POINT('',(9.65,4.28626379701574E-17,0.9));
#13753=CARTESIAN_POINT('',(9.65,4.28626379701574E-17,1.));
#13754=CARTESIAN_POINT('Origin',(10.,0.,0.9));
#13755=CARTESIAN_POINT('Origin',(9.,1.,0.7));
#13756=CARTESIAN_POINT('',(8.75,1.,0.7));
#13757=CARTESIAN_POINT('Origin',(9.,1.,0.7));
#13758=CARTESIAN_POINT('',(8.85,1.,0.7));
#13759=CARTESIAN_POINT('Origin',(9.,1.,0.7));
#13760=CARTESIAN_POINT('Origin',(9.,1.,0.7));
#13761=CARTESIAN_POINT('',(8.75,1.,0.6));
#13762=CARTESIAN_POINT('Origin',(9.,1.,0.6));
#13763=CARTESIAN_POINT('',(8.75,1.,0.7));
#13764=CARTESIAN_POINT('Origin',(9.,1.,0.6));
#13765=CARTESIAN_POINT('Origin',(3.,-1.,0.7));
#13766=CARTESIAN_POINT('',(2.75,-1.,0.7));
#13767=CARTESIAN_POINT('Origin',(3.,-1.,0.7));
#13768=CARTESIAN_POINT('',(2.85,-1.,0.7));
#13769=CARTESIAN_POINT('Origin',(3.,-1.,0.7));
#13770=CARTESIAN_POINT('Origin',(3.,-1.,0.7));
#13771=CARTESIAN_POINT('',(2.75,-1.,0.6));
#13772=CARTESIAN_POINT('Origin',(3.,-1.,0.6));
#13773=CARTESIAN_POINT('',(2.75,-1.,0.7));
#13774=CARTESIAN_POINT('Origin',(3.,-1.,0.6));
#13775=CARTESIAN_POINT('Origin',(3.,1.,0.7));
#13776=CARTESIAN_POINT('',(2.75,1.,0.7));
#13777=CARTESIAN_POINT('Origin',(3.,1.,0.7));
#13778=CARTESIAN_POINT('',(2.85,1.,0.7));
#13779=CARTESIAN_POINT('Origin',(3.,1.,0.7));
#13780=CARTESIAN_POINT('Origin',(3.,1.,0.7));
#13781=CARTESIAN_POINT('',(2.75,1.,0.6));
#13782=CARTESIAN_POINT('Origin',(3.,1.,0.6));
#13783=CARTESIAN_POINT('',(2.75,1.,0.7));
#13784=CARTESIAN_POINT('Origin',(3.,1.,0.6));
#13785=CARTESIAN_POINT('Origin',(9.,-1.,0.7));
#13786=CARTESIAN_POINT('',(8.75,-1.,0.7));
#13787=CARTESIAN_POINT('Origin',(9.,-1.,0.7));
#13788=CARTESIAN_POINT('',(8.85,-1.,0.7));
#13789=CARTESIAN_POINT('Origin',(9.,-1.,0.7));
#13790=CARTESIAN_POINT('Origin',(9.,-1.,0.7));
#13791=CARTESIAN_POINT('',(8.75,-1.,0.6));
#13792=CARTESIAN_POINT('Origin',(9.,-1.,0.6));
#13793=CARTESIAN_POINT('',(8.75,-1.,0.7));
#13794=CARTESIAN_POINT('Origin',(9.,-1.,0.6));
#13795=CARTESIAN_POINT('Origin',(9.,1.,0.9));
#13796=CARTESIAN_POINT('',(8.85,1.,0.9));
#13797=CARTESIAN_POINT('',(8.85,1.,0.9));
#13798=CARTESIAN_POINT('Origin',(9.,1.,0.9));
#13799=CARTESIAN_POINT('Origin',(3.,-1.,0.9));
#13800=CARTESIAN_POINT('',(2.85,-1.,0.9));
#13801=CARTESIAN_POINT('',(2.85,-1.,0.9));
#13802=CARTESIAN_POINT('Origin',(3.,-1.,0.9));
#13803=CARTESIAN_POINT('Origin',(3.,1.,0.9));
#13804=CARTESIAN_POINT('',(2.85,1.,0.9));
#13805=CARTESIAN_POINT('',(2.85,1.,0.9));
#13806=CARTESIAN_POINT('Origin',(3.,1.,0.9));
#13807=CARTESIAN_POINT('Origin',(9.,-1.,0.9));
#13808=CARTESIAN_POINT('',(8.85,-1.,0.9));
#13809=CARTESIAN_POINT('',(8.85,-1.,0.9));
#13810=CARTESIAN_POINT('Origin',(9.,-1.,0.9));
#13811=CARTESIAN_POINT('Ctrl Pts',(11.5038445323837,1.18103800495499,1.1));
#13812=CARTESIAN_POINT('Ctrl Pts',(11.5184054935931,1.17950950960121,1.1));
#13813=CARTESIAN_POINT('Ctrl Pts',(11.5512741038969,1.16492409601325,1.1));
#13814=CARTESIAN_POINT('Ctrl Pts',(11.5664342774515,1.13103804392606,1.1));
#13815=CARTESIAN_POINT('Ctrl Pts',(11.5664342774515,1.11151675574496,1.1));
#13816=CARTESIAN_POINT('Ctrl Pts',(11.5062520964801,1.2039732708886,1.1));
#13817=CARTESIAN_POINT('Ctrl Pts',(11.5256097704488,1.20178950015253,1.09999449529541));
#13818=CARTESIAN_POINT('Ctrl Pts',(11.5690795528293,1.18226331832779,1.09998611288251));
#13819=CARTESIAN_POINT('Ctrl Pts',(11.5893469235372,1.13750635859412,1.09999170314796));
#13820=CARTESIAN_POINT('Ctrl Pts',(11.5895723566779,1.11151675574496,1.1));
#13821=CARTESIAN_POINT('Ctrl Pts',(11.5104252001437,1.2437276609947,1.08142124563721));
#13822=CARTESIAN_POINT('Ctrl Pts',(11.5380451995806,1.2404317701584,1.0816749051734));
#13823=CARTESIAN_POINT('Ctrl Pts',(11.5998825216457,1.21232138637678,1.08202590066027));
#13824=CARTESIAN_POINT('Ctrl Pts',(11.629084458256,1.14864330516641,1.08167049691811));
#13825=CARTESIAN_POINT('Ctrl Pts',(11.629673151989,1.11151675574496,1.08129017730416));
#13826=CARTESIAN_POINT('Ctrl Pts',(11.5120790720623,1.25948300155991,1.0418569252725));
#13827=CARTESIAN_POINT('Ctrl Pts',(11.5430287132786,1.25602537746711,1.04251419789099));
#13828=CARTESIAN_POINT('Ctrl Pts',(11.6126593164611,1.22478248685392,1.04343302714342));
#13829=CARTESIAN_POINT('Ctrl Pts',(11.6451104499416,1.15305025146974,1.04249969645955));
#13830=CARTESIAN_POINT('Ctrl Pts',(11.6454164251054,1.11151675574496,1.0415166534692));
#13831=CARTESIAN_POINT('Ctrl Pts',(11.5121826600865,1.26046981594516,1.0245894475956));
#13832=CARTESIAN_POINT('Ctrl Pts',(11.5433440226796,1.25715387309455,1.02536599531596));
#13833=CARTESIAN_POINT('Ctrl Pts',(11.6137195683385,1.22584236729999,1.02645725900057));
#13834=CARTESIAN_POINT('Ctrl Pts',(11.6462638499073,1.15328744881755,1.02534682499181));
#13835=CARTESIAN_POINT('Ctrl Pts',(11.6463246402318,1.11151675574496,1.02418687649944));
#13836=CARTESIAN_POINT('',(11.5664342774515,1.11151675574496,1.1));
#13837=CARTESIAN_POINT('',(11.6463246402318,1.11151675574496,1.02418687649943));
#13838=CARTESIAN_POINT('Origin',(11.5664342774515,1.11151675574496,1.02));
#13839=CARTESIAN_POINT('',(11.5121826600865,1.26046981594516,1.0245894475956));
#13840=CARTESIAN_POINT('Ctrl Pts',(11.6463246402318,1.11151675574496,1.02418687649944));
#13841=CARTESIAN_POINT('Ctrl Pts',(11.6462638499073,1.15328744881755,1.02534682499181));
#13842=CARTESIAN_POINT('Ctrl Pts',(11.6137195683385,1.22584236729999,1.02645725900057));
#13843=CARTESIAN_POINT('Ctrl Pts',(11.5433440226796,1.25715387309455,1.02536599531596));
#13844=CARTESIAN_POINT('Ctrl Pts',(11.5121826600865,1.26046981594516,1.0245894475956));
#13845=CARTESIAN_POINT('',(11.5038445323837,1.18103800495499,1.1));
#13846=CARTESIAN_POINT('Origin',(11.5038445323837,1.18103800495499,1.02));
#13847=CARTESIAN_POINT('Ctrl Pts',(11.5038445323837,1.18103800495499,1.1));
#13848=CARTESIAN_POINT('Ctrl Pts',(11.5184054935931,1.17950950960121,1.1));
#13849=CARTESIAN_POINT('Ctrl Pts',(11.5512741038969,1.16492409601325,1.1));
#13850=CARTESIAN_POINT('Ctrl Pts',(11.5664342774515,1.13103804392606,1.1));
#13851=CARTESIAN_POINT('Ctrl Pts',(11.5664342774515,1.11151675574496,1.1));
#13852=CARTESIAN_POINT('Origin',(11.5664342774515,0.626416499322631,1.02));
#13853=CARTESIAN_POINT('',(11.5664342774515,-1.11151675574496,1.1));
#13854=CARTESIAN_POINT('',(11.6463246402318,-1.11151675574496,1.02418687649944));
#13855=CARTESIAN_POINT('Origin',(11.5664342774515,-1.11151675574496,1.02));
#13856=CARTESIAN_POINT('',(11.6463246402318,0.626416499322631,1.02418687649944));
#13857=CARTESIAN_POINT('',(11.5664342774515,0.626416499322631,1.1));
#13858=CARTESIAN_POINT('Ctrl Pts',(11.5664342774515,-1.11151675574496,1.1));
#13859=CARTESIAN_POINT('Ctrl Pts',(11.5664342774515,-1.12615772189446,1.1));
#13860=CARTESIAN_POINT('Ctrl Pts',(11.5553715698491,-1.16037133170262,1.1));
#13861=CARTESIAN_POINT('Ctrl Pts',(11.5232591473477,-1.17900001114805,1.1));
#13862=CARTESIAN_POINT('Ctrl Pts',(11.5038445323837,-1.181038004955,1.1));
#13863=CARTESIAN_POINT('Ctrl Pts',(11.5895723566779,-1.11151675574496,1.1));
#13864=CARTESIAN_POINT('Ctrl Pts',(11.5894032818222,-1.13100895790003,1.09999377736097));
#13865=CARTESIAN_POINT('Ctrl Pts',(11.5744722352599,-1.17628172883974,1.09998542409303));
#13866=CARTESIAN_POINT('Ctrl Pts',(11.5320623284624,-1.20106157657112,1.09999266039387));
#13867=CARTESIAN_POINT('Ctrl Pts',(11.5062520964801,-1.2039732708886,1.1));
#13868=CARTESIAN_POINT('Ctrl Pts',(11.6296731519891,-1.11151675574496,1.0812901773042));
#13869=CARTESIAN_POINT('Ctrl Pts',(11.6292316316889,-1.13936166783705,1.08157541701493));
#13870=CARTESIAN_POINT('Ctrl Pts',(11.6075809177182,-1.20379599023677,1.08201780166247));
#13871=CARTESIAN_POINT('Ctrl Pts',(11.547251866094,-1.23933313987557,1.08175945835248));
#13872=CARTESIAN_POINT('Ctrl Pts',(11.5104252001437,-1.24372766099475,1.08142124563725));
#13873=CARTESIAN_POINT('Ctrl Pts',(11.6454164251054,-1.11151675574496,1.0415166534692));
#13874=CARTESIAN_POINT('Ctrl Pts',(11.6451869437323,-1.14266687756763,1.04225393571265));
#13875=CARTESIAN_POINT('Ctrl Pts',(11.6213248916312,-1.21516855113593,1.04341114660737));
#13876=CARTESIAN_POINT('Ctrl Pts',(11.5533452603892,-1.25487283609854,1.04273328876464));
#13877=CARTESIAN_POINT('Ctrl Pts',(11.5120790720623,-1.25948300155991,1.0418569252725));
#13878=CARTESIAN_POINT('Ctrl Pts',(11.6463246402318,-1.11151675574496,1.02418687649944));
#13879=CARTESIAN_POINT('Ctrl Pts',(11.6462790474884,-1.14284477557865,1.02505683786953));
#13880=CARTESIAN_POINT('Ctrl Pts',(11.6225012384517,-1.21608782625165,1.02643081388051));
#13881=CARTESIAN_POINT('Ctrl Pts',(11.5537311435827,-1.25604855880689,1.02562484455705));
#13882=CARTESIAN_POINT('Ctrl Pts',(11.5121826600865,-1.26046981594517,1.0245894475956));
#13883=CARTESIAN_POINT('',(11.5038445323837,-1.181038004955,1.1));
#13884=CARTESIAN_POINT('',(11.5121826600865,-1.26046981594517,1.02458944759559));
#13885=CARTESIAN_POINT('Origin',(11.5038445323837,-1.181038004955,1.02));
#13886=CARTESIAN_POINT('Ctrl Pts',(11.5121826600865,-1.26046981594517,1.0245894475956));
#13887=CARTESIAN_POINT('Ctrl Pts',(11.5537311435827,-1.25604855880689,1.02562484455705));
#13888=CARTESIAN_POINT('Ctrl Pts',(11.6225012384517,-1.21608782625165,1.02643081388051));
#13889=CARTESIAN_POINT('Ctrl Pts',(11.6462790474884,-1.14284477557865,1.02505683786953));
#13890=CARTESIAN_POINT('Ctrl Pts',(11.6463246402318,-1.11151675574496,1.02418687649944));
#13891=CARTESIAN_POINT('Ctrl Pts',(11.5664342774515,-1.11151675574496,1.1));
#13892=CARTESIAN_POINT('Ctrl Pts',(11.5664342774515,-1.12615772189446,1.1));
#13893=CARTESIAN_POINT('Ctrl Pts',(11.5553715698491,-1.16037133170262,1.1));
#13894=CARTESIAN_POINT('Ctrl Pts',(11.5232591473477,-1.17900001114805,1.1));
#13895=CARTESIAN_POINT('Ctrl Pts',(11.5038445323837,-1.181038004955,1.1));
#13896=CARTESIAN_POINT('Ctrl Pts',(11.5038445323836,-1.181038004955,1.1));
#13897=CARTESIAN_POINT('Ctrl Pts',(9.93221394244152,-1.34601544154236,1.1));
#13898=CARTESIAN_POINT('Ctrl Pts',(7.3047417451522,-1.56119993769491,1.1));
#13899=CARTESIAN_POINT('Ctrl Pts',(3.61332606662357,-1.48882378722464,1.1));
#13900=CARTESIAN_POINT('Ctrl Pts',(1.52093096174237,-1.20661833758759,1.1));
#13901=CARTESIAN_POINT('Ctrl Pts',(0.489277774073836,-0.993132359214002,
1.1));
#13902=CARTESIAN_POINT('Ctrl Pts',(11.5062520964801,-1.2039732708886,1.1));
#13903=CARTESIAN_POINT('Ctrl Pts',(9.93427206726409,-1.36902193231914,1.10000125302342));
#13904=CARTESIAN_POINT('Ctrl Pts',(7.30574352860662,-1.58436797372637,1.10000007151586));
#13905=CARTESIAN_POINT('Ctrl Pts',(3.61166276511536,-1.51194672535434,1.09999968963322));
#13906=CARTESIAN_POINT('Ctrl Pts',(1.51730587435546,-1.22941181706429,1.10000211650891));
#13907=CARTESIAN_POINT('Ctrl Pts',(0.48461766586479,-1.01565194352286,1.1));
#13908=CARTESIAN_POINT('Ctrl Pts',(11.5104252017938,-1.24372767671385,1.08142125970198));
#13909=CARTESIAN_POINT('Ctrl Pts',(9.93784299858723,-1.40889527428921,1.08136351975694));
#13910=CARTESIAN_POINT('Ctrl Pts',(7.3074712357333,-1.62451940065184,1.08127113650551));
#13911=CARTESIAN_POINT('Ctrl Pts',(3.60878747433083,-1.55202277432172,1.08130174433006));
#13912=CARTESIAN_POINT('Ctrl Pts',(1.51101154909588,-1.26891547398152,1.08143311272106));
#13913=CARTESIAN_POINT('Ctrl Pts',(0.476539293980871,-1.05469000198791,
1.08153107638517));
#13914=CARTESIAN_POINT('Ctrl Pts',(11.5120790720622,-1.25948300155992,1.0418569252725));
#13915=CARTESIAN_POINT('Ctrl Pts',(9.93924961011084,-1.42463380902671,1.04170731179674));
#13916=CARTESIAN_POINT('Ctrl Pts',(7.30815001459807,-1.64026117966461,1.0414672686166));
#13917=CARTESIAN_POINT('Ctrl Pts',(3.60765874156876,-1.56776897899067,1.04154646081959));
#13918=CARTESIAN_POINT('Ctrl Pts',(1.50852499534242,-1.28458904017411,1.04188830921359));
#13919=CARTESIAN_POINT('Ctrl Pts',(0.473312455428654,-1.07028343020201,
1.04214267388586));
#13920=CARTESIAN_POINT('Ctrl Pts',(11.5121826600865,-1.26046981594517,1.0245894475956));
#13921=CARTESIAN_POINT('Ctrl Pts',(9.9393350416019,-1.42558521977072,1.02441268379886));
#13922=CARTESIAN_POINT('Ctrl Pts',(7.30818539134325,-1.64115782448209,1.02412850358181));
#13923=CARTESIAN_POINT('Ctrl Pts',(3.607597182252,-1.56868448653922,1.02422201615766));
#13924=CARTESIAN_POINT('Ctrl Pts',(1.50836811330665,-1.28557739750152,1.02462705425916));
#13925=CARTESIAN_POINT('Ctrl Pts',(0.473097162761967,-1.07132381406029,
1.02492790083044));
#13926=CARTESIAN_POINT('',(0.489277774073836,-0.993132359214002,1.1));
#13927=CARTESIAN_POINT('',(0.473097162761967,-1.07132381406029,1.02492790083044));
#13928=CARTESIAN_POINT('Origin',(0.489277774073836,-0.993132359214002,1.02));
#13929=CARTESIAN_POINT('Ctrl Pts',(0.473097162761967,-1.07132381406029,
1.02492790083044));
#13930=CARTESIAN_POINT('Ctrl Pts',(1.50836811330665,-1.28557739750152,1.02462705425916));
#13931=CARTESIAN_POINT('Ctrl Pts',(3.607597182252,-1.56868448653922,1.02422201615766));
#13932=CARTESIAN_POINT('Ctrl Pts',(7.30818539134325,-1.64115782448209,1.02412850358181));
#13933=CARTESIAN_POINT('Ctrl Pts',(9.9393350416019,-1.42558521977072,1.02441268379886));
#13934=CARTESIAN_POINT('Ctrl Pts',(11.5121826600865,-1.26046981594517,1.0245894475956));
#13935=CARTESIAN_POINT('Ctrl Pts',(11.5038445323836,-1.181038004955,1.1));
#13936=CARTESIAN_POINT('Ctrl Pts',(9.93221394244152,-1.34601544154236,1.1));
#13937=CARTESIAN_POINT('Ctrl Pts',(7.3047417451522,-1.56119993769491,1.1));
#13938=CARTESIAN_POINT('Ctrl Pts',(3.61332606662357,-1.48882378722464,1.1));
#13939=CARTESIAN_POINT('Ctrl Pts',(1.52093096174237,-1.20661833758759,1.1));
#13940=CARTESIAN_POINT('Ctrl Pts',(0.489277774073836,-0.993132359214002,
1.1));
#13941=CARTESIAN_POINT('Ctrl Pts',(0.489277774073836,-0.993132359214003,
1.1));
#13942=CARTESIAN_POINT('Ctrl Pts',(0.47591459116406,-0.990367038259462,
1.1));
#13943=CARTESIAN_POINT('Ctrl Pts',(0.446638556739065,-0.974524902741032,
1.1));
#13944=CARTESIAN_POINT('Ctrl Pts',(0.433565722548535,-0.942876078073176,
1.1));
#13945=CARTESIAN_POINT('Ctrl Pts',(0.433565722548535,-0.924681003894255,
1.1));
#13946=CARTESIAN_POINT('Ctrl Pts',(0.48461766586479,-1.01565194352286,1.1));
#13947=CARTESIAN_POINT('Ctrl Pts',(0.466871946563175,-1.01185427439077,
1.09999555360656));
#13948=CARTESIAN_POINT('Ctrl Pts',(0.428148998320346,-0.990723083341879,
1.0999884677795));
#13949=CARTESIAN_POINT('Ctrl Pts',(0.410637366989639,-0.948905017863894,
1.09999228132016));
#13950=CARTESIAN_POINT('Ctrl Pts',(0.410427643322096,-0.924681003894255,
1.1));
#13951=CARTESIAN_POINT('Ctrl Pts',(0.47653584926364,-1.05470664829667,1.08154627613271));
#13952=CARTESIAN_POINT('Ctrl Pts',(0.451238756159369,-1.04914377880765,
1.08175207965746));
#13953=CARTESIAN_POINT('Ctrl Pts',(0.396142217510869,-1.01881823177681,
1.08201099971769));
#13954=CARTESIAN_POINT('Ctrl Pts',(0.370857020273576,-0.959285462196374,
1.08165947596025));
#13955=CARTESIAN_POINT('Ctrl Pts',(0.370309350093454,-0.924681003894255,
1.0813056591965));
#13956=CARTESIAN_POINT('Ctrl Pts',(0.473312455428654,-1.07028343020201,
1.04214267388586));
#13957=CARTESIAN_POINT('Ctrl Pts',(0.444929265438756,-1.064235408557,1.04267704697817));
#13958=CARTESIAN_POINT('Ctrl Pts',(0.382898223041383,-1.03040761468413,
1.04335444671884));
#13959=CARTESIAN_POINT('Ctrl Pts',(0.354868227955524,-0.963393056722486,
1.04243119239046));
#13960=CARTESIAN_POINT('Ctrl Pts',(0.354583574894625,-0.924681003894255,
1.0415166534692));
#13961=CARTESIAN_POINT('Ctrl Pts',(0.473097162761967,-1.07132381406029,
1.02492790083044));
#13962=CARTESIAN_POINT('Ctrl Pts',(0.444494893732137,-1.06536514830602,
1.02555992378854));
#13963=CARTESIAN_POINT('Ctrl Pts',(0.381802689524125,-1.03137574421946,
1.02636429433614));
#13964=CARTESIAN_POINT('Ctrl Pts',(0.353731913874551,-0.963614141904928,
1.02526599313355));
#13965=CARTESIAN_POINT('Ctrl Pts',(0.35367535976817,-0.924681003894255,
1.02418687649944));
#13966=CARTESIAN_POINT('',(0.433565722548535,-0.924681003894255,1.1));
#13967=CARTESIAN_POINT('',(0.35367535976817,-0.924681003894255,1.02418687649944));
#13968=CARTESIAN_POINT('Origin',(0.433565722548536,-0.924681003894255,1.02));
#13969=CARTESIAN_POINT('Ctrl Pts',(0.35367535976817,-0.924681003894255,
1.02418687649944));
#13970=CARTESIAN_POINT('Ctrl Pts',(0.353731913874551,-0.963614141904928,
1.02526599313355));
#13971=CARTESIAN_POINT('Ctrl Pts',(0.381802689524125,-1.03137574421946,
1.02636429433614));
#13972=CARTESIAN_POINT('Ctrl Pts',(0.444494893732137,-1.06536514830602,
1.02555992378854));
#13973=CARTESIAN_POINT('Ctrl Pts',(0.473097162761967,-1.07132381406029,
1.02492790083044));
#13974=CARTESIAN_POINT('Ctrl Pts',(0.489277774073836,-0.993132359214003,
1.1));
#13975=CARTESIAN_POINT('Ctrl Pts',(0.47591459116406,-0.990367038259462,
1.1));
#13976=CARTESIAN_POINT('Ctrl Pts',(0.446638556739065,-0.974524902741032,
1.1));
#13977=CARTESIAN_POINT('Ctrl Pts',(0.433565722548535,-0.942876078073176,
1.1));
#13978=CARTESIAN_POINT('Ctrl Pts',(0.433565722548535,-0.924681003894255,
1.1));
#13979=CARTESIAN_POINT('Origin',(0.433565722548536,-0.526416499322631,1.02));
#13980=CARTESIAN_POINT('',(0.433565722548536,0.924681003894255,1.1));
#13981=CARTESIAN_POINT('',(0.35367535976817,0.924681003894255,1.02418687649944));
#13982=CARTESIAN_POINT('Origin',(0.433565722548536,0.924681003894255,1.02));
#13983=CARTESIAN_POINT('',(0.35367535976817,-0.526416499322631,1.02418687649944));
#13984=CARTESIAN_POINT('',(0.433565722548536,-0.526416499322631,1.1));
#13985=CARTESIAN_POINT('Ctrl Pts',(0.433565722548535,0.924681003894255,
1.1));
#13986=CARTESIAN_POINT('Ctrl Pts',(0.433565722548535,0.94287607801605,1.1));
#13987=CARTESIAN_POINT('Ctrl Pts',(0.44664012289244,0.97452669098104,1.1));
#13988=CARTESIAN_POINT('Ctrl Pts',(0.475914591206016,0.990367038268144,
1.1));
#13989=CARTESIAN_POINT('Ctrl Pts',(0.489277774073836,0.993132359214003,
1.1));
#13990=CARTESIAN_POINT('Ctrl Pts',(0.410427643322096,0.924681003894255,
1.1));
#13991=CARTESIAN_POINT('Ctrl Pts',(0.410637366988981,0.948905017787839,
1.09999228132018));
#13992=CARTESIAN_POINT('Ctrl Pts',(0.428151078432557,0.99072545440496,1.09998846767325));
#13993=CARTESIAN_POINT('Ctrl Pts',(0.466871946618891,1.01185427440269,1.09999555360657));
#13994=CARTESIAN_POINT('Ctrl Pts',(0.48461766586479,1.01565194352286,1.1));
#13995=CARTESIAN_POINT('Ctrl Pts',(0.370309350093454,0.924681003894255,
1.0813056591965));
#13996=CARTESIAN_POINT('Ctrl Pts',(0.370857020271857,0.959285462087728,
1.08165947595914));
#13997=CARTESIAN_POINT('Ctrl Pts',(0.396145183504025,1.01882160767722,1.08201100382378));
#13998=CARTESIAN_POINT('Ctrl Pts',(0.451238756238795,1.04914377882512,1.08175207965681));
#13999=CARTESIAN_POINT('Ctrl Pts',(0.47653584926364,1.05470664829667,1.08154627613271));
#14000=CARTESIAN_POINT('Ctrl Pts',(0.354583574894625,0.924681003894255,
1.0415166534692));
#14001=CARTESIAN_POINT('Ctrl Pts',(0.35486822795463,0.963393056600943,1.04243119238759));
#14002=CARTESIAN_POINT('Ctrl Pts',(0.382901552879886,1.03041141096935,1.04335445746542));
#14003=CARTESIAN_POINT('Ctrl Pts',(0.444929265527871,1.06423540857599,1.04267704697649));
#14004=CARTESIAN_POINT('Ctrl Pts',(0.473312455428654,1.07028343020201,1.04214267388586));
#14005=CARTESIAN_POINT('Ctrl Pts',(0.35367535976817,0.924681003894255,1.02418687649944));
#14006=CARTESIAN_POINT('Ctrl Pts',(0.353731913874373,0.963614141782691,
1.02526599313016));
#14007=CARTESIAN_POINT('Ctrl Pts',(0.381806046235973,1.03137957549636,1.02636430709951));
#14008=CARTESIAN_POINT('Ctrl Pts',(0.44449489382194,1.06536514832473,1.02555992378656));
#14009=CARTESIAN_POINT('Ctrl Pts',(0.473097162761967,1.07132381406029,1.02492790083044));
#14010=CARTESIAN_POINT('',(0.489277774073836,0.993132359214003,1.1));
#14011=CARTESIAN_POINT('',(0.473097162761967,1.07132381406029,1.02492790083044));
#14012=CARTESIAN_POINT('Origin',(0.489277774073836,0.993132359214003,1.02));
#14013=CARTESIAN_POINT('Ctrl Pts',(0.473097162761967,1.07132381406029,1.02492790083044));
#14014=CARTESIAN_POINT('Ctrl Pts',(0.44449489382194,1.06536514832473,1.02555992378656));
#14015=CARTESIAN_POINT('Ctrl Pts',(0.381806046235973,1.03137957549636,1.02636430709951));
#14016=CARTESIAN_POINT('Ctrl Pts',(0.353731913874373,0.963614141782691,
1.02526599313016));
#14017=CARTESIAN_POINT('Ctrl Pts',(0.35367535976817,0.924681003894255,1.02418687649944));
#14018=CARTESIAN_POINT('Ctrl Pts',(0.433565722548535,0.924681003894255,
1.1));
#14019=CARTESIAN_POINT('Ctrl Pts',(0.433565722548535,0.94287607801605,1.1));
#14020=CARTESIAN_POINT('Ctrl Pts',(0.44664012289244,0.97452669098104,1.1));
#14021=CARTESIAN_POINT('Ctrl Pts',(0.475914591206016,0.990367038268144,
1.1));
#14022=CARTESIAN_POINT('Ctrl Pts',(0.489277774073836,0.993132359214003,
1.1));
#14023=CARTESIAN_POINT('Ctrl Pts',(0.489277774073836,0.993132359214003,
1.1));
#14024=CARTESIAN_POINT('Ctrl Pts',(1.52092917355268,1.20661796754713,1.1));
#14025=CARTESIAN_POINT('Ctrl Pts',(3.61335021200387,1.48882484395407,1.1));
#14026=CARTESIAN_POINT('Ctrl Pts',(7.30471495328446,1.56119985233321,1.1));
#14027=CARTESIAN_POINT('Ctrl Pts',(9.93221666658724,1.34601515558293,1.1));
#14028=CARTESIAN_POINT('Ctrl Pts',(11.5038445323836,1.18103800495499,1.1));
#14029=CARTESIAN_POINT('Ctrl Pts',(0.48461766586479,1.01565194352286,1.1));
#14030=CARTESIAN_POINT('Ctrl Pts',(1.51730408437175,1.22941144654908,1.10000211650524));
#14031=CARTESIAN_POINT('Ctrl Pts',(3.61168692820091,1.5119477834436,1.09999968963693));
#14032=CARTESIAN_POINT('Ctrl Pts',(7.30571671988008,1.58436788793099,1.10000007151498));
#14033=CARTESIAN_POINT('Ctrl Pts',(9.9342747920155,1.36902164623626,1.10000125302125));
#14034=CARTESIAN_POINT('Ctrl Pts',(11.5062520964801,1.2039732708886,1.1));
#14035=CARTESIAN_POINT('Ctrl Pts',(0.476539293980872,1.05469000198791,1.08153107638517));
#14036=CARTESIAN_POINT('Ctrl Pts',(1.51100975601983,1.26891510265927,1.08143311289086));
#14037=CARTESIAN_POINT('Ctrl Pts',(3.60881166804804,1.5520238347382,1.08130174382265));
#14038=CARTESIAN_POINT('Ctrl Pts',(7.30744439783659,1.62451931411139,1.08127113658549));
#14039=CARTESIAN_POINT('Ctrl Pts',(9.9378457243824,1.40889498800017,1.08136351985702));
#14040=CARTESIAN_POINT('Ctrl Pts',(11.5104252017938,1.24372767671385,1.08142125970198));
#14041=CARTESIAN_POINT('Ctrl Pts',(0.473312455428654,1.07028343020201,1.04214267388586));
#14042=CARTESIAN_POINT('Ctrl Pts',(1.50852320098322,1.28458866871296,1.04188830965449));
#14043=CARTESIAN_POINT('Ctrl Pts',(3.60768294746331,1.5677700397583,1.04154645950336));
#14044=CARTESIAN_POINT('Ctrl Pts',(7.30812316513016,1.64026109291585,1.04146726882447));
#14045=CARTESIAN_POINT('Ctrl Pts',(9.93925233633459,1.42463352276678,1.04170731205607));
#14046=CARTESIAN_POINT('Ctrl Pts',(11.5120790720622,1.25948300155991,1.0418569252725));
#14047=CARTESIAN_POINT('Ctrl Pts',(0.473097162761967,1.07132381406029,1.02492790083044));
#14048=CARTESIAN_POINT('Ctrl Pts',(1.50836631884621,1.28557702613055,1.02462705478063));
#14049=CARTESIAN_POINT('Ctrl Pts',(3.60762138890097,1.56868554702656,1.02422201460129));
#14050=CARTESIAN_POINT('Ctrl Pts',(7.30815854116978,1.64115773776738,1.02412850382783));
#14051=CARTESIAN_POINT('Ctrl Pts',(9.93933776785713,1.42558493357216,1.02441268410525));
#14052=CARTESIAN_POINT('Ctrl Pts',(11.5121826600865,1.26046981594517,1.0245894475956));
#14053=CARTESIAN_POINT('Ctrl Pts',(11.5121826600865,1.26046981594517,1.0245894475956));
#14054=CARTESIAN_POINT('Ctrl Pts',(9.93933776785713,1.42558493357216,1.02441268410525));
#14055=CARTESIAN_POINT('Ctrl Pts',(7.30815854116978,1.64115773776738,1.02412850382783));
#14056=CARTESIAN_POINT('Ctrl Pts',(3.60762138890097,1.56868554702656,1.02422201460129));
#14057=CARTESIAN_POINT('Ctrl Pts',(1.50836631884621,1.28557702613055,1.02462705478063));
#14058=CARTESIAN_POINT('Ctrl Pts',(0.473097162761967,1.07132381406029,1.02492790083044));
#14059=CARTESIAN_POINT('Ctrl Pts',(0.489277774073836,0.993132359214003,
1.1));
#14060=CARTESIAN_POINT('Ctrl Pts',(1.52092917355268,1.20661796754713,1.1));
#14061=CARTESIAN_POINT('Ctrl Pts',(3.61335021200387,1.48882484395407,1.1));
#14062=CARTESIAN_POINT('Ctrl Pts',(7.30471495328446,1.56119985233321,1.1));
#14063=CARTESIAN_POINT('Ctrl Pts',(9.93221666658724,1.34601515558293,1.1));
#14064=CARTESIAN_POINT('Ctrl Pts',(11.5038445323836,1.18103800495499,1.1));
#14065=CARTESIAN_POINT('Origin',(0.347167001354737,-1.05283299864526,0.9));
#14066=CARTESIAN_POINT('',(0.347167001354737,0.931160914046453,0.9));
#14067=CARTESIAN_POINT('Ctrl Pts',(0.347167001354737,0.931160914046453,
0.9));
#14068=CARTESIAN_POINT('Ctrl Pts',(0.34933645413337,0.929000934518636,0.941395625006663));
#14069=CARTESIAN_POINT('Ctrl Pts',(0.351505906937822,0.926840964458487,
0.982791250505987));
#14070=CARTESIAN_POINT('Ctrl Pts',(0.35367535976817,0.924681003894255,1.02418687649944));
#14071=CARTESIAN_POINT('',(0.347167001354737,-0.931160914046453,0.9));
#14072=CARTESIAN_POINT('',(0.347167001354737,-1.05283299864526,0.9));
#14073=CARTESIAN_POINT('Ctrl Pts',(0.35367535976817,-0.924681003894255,
1.02418687649944));
#14074=CARTESIAN_POINT('Ctrl Pts',(0.351505906937822,-0.926840964458487,
0.982791250505987));
#14075=CARTESIAN_POINT('Ctrl Pts',(0.34933645413337,-0.929000934518636,
0.941395625006663));
#14076=CARTESIAN_POINT('Ctrl Pts',(0.347167001354737,-0.931160914046453,
0.9));
#14077=CARTESIAN_POINT('Ctrl Pts',(0.346994979645257,0.93133218461645,0.89671763024815));
#14078=CARTESIAN_POINT('Ctrl Pts',(0.349221772992334,0.929115114391563,
0.939207378479044));
#14079=CARTESIAN_POINT('Ctrl Pts',(0.35144856636661,0.926898054140648,0.981697127228945));
#14080=CARTESIAN_POINT('Ctrl Pts',(0.35367535976817,0.924681003894255,1.02418687649944));
#14081=CARTESIAN_POINT('Ctrl Pts',(0.347101141748081,0.970260862175626,
0.898743323843195));
#14082=CARTESIAN_POINT('Ctrl Pts',(0.349327989245423,0.968041585482289,
0.94123294798136));
#14083=CARTESIAN_POINT('Ctrl Pts',(0.35155465541633,0.96582239703375,0.983722586263841));
#14084=CARTESIAN_POINT('Ctrl Pts',(0.353781503060223,0.96360313540272,1.02621221116359));
#14085=CARTESIAN_POINT('Ctrl Pts',(0.375231247034764,1.03797686888013,0.90080243726586));
#14086=CARTESIAN_POINT('Ctrl Pts',(0.377454726329371,1.03575393200526,0.943292036336267));
#14087=CARTESIAN_POINT('Ctrl Pts',(0.379678256934949,1.03353096064141,0.985781630873016));
#14088=CARTESIAN_POINT('Ctrl Pts',(0.381901729528225,1.03130803054038,1.02827123060239));
#14089=CARTESIAN_POINT('Ctrl Pts',(0.437891832981715,1.07196344732884,0.899291918906528));
#14090=CARTESIAN_POINT('Ctrl Pts',(0.440109459023804,1.06974216787274,0.941781905864285));
#14091=CARTESIAN_POINT('Ctrl Pts',(0.442327107866739,1.06752094195844,0.984271894420663));
#14092=CARTESIAN_POINT('Ctrl Pts',(0.44454471435444,1.06529967134173,1.02676188280081));
#14093=CARTESIAN_POINT('Ctrl Pts',(0.466484255634356,1.07794817238022,0.898105730168711));
#14094=CARTESIAN_POINT('Ctrl Pts',(0.46869984010673,1.07572875745303,0.940595920481163));
#14095=CARTESIAN_POINT('Ctrl Pts',(0.470915412358444,1.07350934859911,0.983086111716909));
#14096=CARTESIAN_POINT('Ctrl Pts',(0.473130972350001,1.07128994583173,1.02557630387858));
#14097=CARTESIAN_POINT('',(0.466583029361855,1.07784922788182,0.9));
#14098=CARTESIAN_POINT('Ctrl Pts',(0.473097162761967,1.07132381406029,1.02492790083044));
#14099=CARTESIAN_POINT('Ctrl Pts',(0.470925796725269,1.07349894615889,0.983285266331776));
#14100=CARTESIAN_POINT('Ctrl Pts',(0.468754418912838,1.07567408410356,0.941642632722456));
#14101=CARTESIAN_POINT('Ctrl Pts',(0.466583029361855,1.07784922788182,0.9));
#14102=CARTESIAN_POINT('Ctrl Pts',(0.466583029361856,1.07784922788182,0.9));
#14103=CARTESIAN_POINT('Ctrl Pts',(0.45605169130101,1.07567238924625,0.899999999995368));
#14104=CARTESIAN_POINT('Ctrl Pts',(0.445810809951917,1.07234818111891,0.899998625774342));
#14105=CARTESIAN_POINT('Ctrl Pts',(0.436024610942277,1.06798890472683,0.899998407511246));
#14106=CARTESIAN_POINT('Ctrl Pts',(0.42804650025127,1.0644350438709,0.899998229574221));
#14107=CARTESIAN_POINT('Ctrl Pts',(0.420370119207661,1.06019193848671,0.899998775177391));
#14108=CARTESIAN_POINT('Ctrl Pts',(0.413095080427888,1.05529723033767,0.89999964722522));
#14109=CARTESIAN_POINT('Ctrl Pts',(0.404948343152914,1.04981603600524,0.900000623762221));
#14110=CARTESIAN_POINT('Ctrl Pts',(0.3973835293994,1.04357129238854,0.900002055204145));
#14111=CARTESIAN_POINT('Ctrl Pts',(0.390528747317286,1.03663323920468,0.900000884971142));
#14112=CARTESIAN_POINT('Ctrl Pts',(0.38377850537204,1.02980099609921,0.899999732584995));
#14113=CARTESIAN_POINT('Ctrl Pts',(0.377716121663402,1.02229558340178,0.899996048870533));
#14114=CARTESIAN_POINT('Ctrl Pts',(0.372394770625083,1.01423711207676,0.899993306941804));
#14115=CARTESIAN_POINT('Ctrl Pts',(0.366459905306112,1.00524955578769,0.899990248888012));
#14116=CARTESIAN_POINT('Ctrl Pts',(0.361501411166698,0.995658501454654,
0.8999884459165));
#14117=CARTESIAN_POINT('Ctrl Pts',(0.35758177265536,0.985639755107121,0.899989063766683));
#14118=CARTESIAN_POINT('Ctrl Pts',(0.356156017388132,0.981995469968403,
0.8999892885076));
#14119=CARTESIAN_POINT('Ctrl Pts',(0.354868143601992,0.978294337124559,
0.899989797558581));
#14120=CARTESIAN_POINT('Ctrl Pts',(0.353722739999278,0.97454418014098,0.899990530873797));
#14121=CARTESIAN_POINT('Ctrl Pts',(0.350595356382139,0.964304837882626,
0.899992533100777));
#14122=CARTESIAN_POINT('Ctrl Pts',(0.348551371116014,0.953782216732967,
0.899996407005639));
#14123=CARTESIAN_POINT('Ctrl Pts',(0.347666342074759,0.943140644221274,
0.899998614621972));
#14124=CARTESIAN_POINT('Ctrl Pts',(0.347335396628921,0.939161362417926,
0.899999440132251));
#14125=CARTESIAN_POINT('Ctrl Pts',(0.347167001797138,0.935165318330998,
0.899999999966431));
#14126=CARTESIAN_POINT('Ctrl Pts',(0.347167001354737,0.931160914046453,
0.9));
#14127=CARTESIAN_POINT('Ctrl Pts',(0.466583029361855,1.07784922788182,0.9));
#14128=CARTESIAN_POINT('Ctrl Pts',(0.468719324182819,1.07566682993082,0.941642633610146));
#14129=CARTESIAN_POINT('Ctrl Pts',(0.470855619003782,1.07348443197981,0.983285267220292));
#14130=CARTESIAN_POINT('Ctrl Pts',(0.472991913824746,1.07130203402881,1.02492790083044));
#14131=CARTESIAN_POINT('Ctrl Pts',(4.1506201585889,1.83934349355009,0.9));
#14132=CARTESIAN_POINT('Ctrl Pts',(4.15133415151554,1.83716109559909,0.941642633610146));
#14133=CARTESIAN_POINT('Ctrl Pts',(4.15204814444219,1.83497869764808,0.983285267220293));
#14134=CARTESIAN_POINT('Ctrl Pts',(4.15276213736883,1.83279629969708,1.02492790083044));
#14135=CARTESIAN_POINT('Ctrl Pts',(7.83465728781595,1.65326443611903,0.9));
#14136=CARTESIAN_POINT('Ctrl Pts',(7.83394897884827,1.65108203816803,0.941642633610146));
#14137=CARTESIAN_POINT('Ctrl Pts',(7.83324066988059,1.64889964021702,0.983285267220292));
#14138=CARTESIAN_POINT('Ctrl Pts',(7.83253236091292,1.64671724226602,1.02492790083044));
#14139=CARTESIAN_POINT('Ctrl Pts',(11.518694417043,1.26698486563531,0.9));
#14140=CARTESIAN_POINT('Ctrl Pts',(11.516563806181,1.26480246768431,0.941642633610146));
#14141=CARTESIAN_POINT('Ctrl Pts',(11.514433195319,1.2626200697333,0.983285267220292));
#14142=CARTESIAN_POINT('Ctrl Pts',(11.512302584457,1.2604376717823,1.02492790083044));
#14143=CARTESIAN_POINT('',(11.518694417043,1.26698486563531,0.9));
#14144=CARTESIAN_POINT('Ctrl Pts',(11.518694417043,1.26698486563531,0.9));
#14145=CARTESIAN_POINT('Ctrl Pts',(11.5165238247878,1.26481317761477,0.941529815291285));
#14146=CARTESIAN_POINT('Ctrl Pts',(11.5143532391283,1.26264149437998,0.983059631155884));
#14147=CARTESIAN_POINT('Ctrl Pts',(11.5121826600865,1.26046981594516,1.0245894475956));
#14148=CARTESIAN_POINT('Ctrl Pts',(0.466583029361855,1.07784922788182,0.9));
#14149=CARTESIAN_POINT('Ctrl Pts',(4.1506201585889,1.83934349355009,0.9));
#14150=CARTESIAN_POINT('Ctrl Pts',(7.83465728781595,1.65326443611903,0.9));
#14151=CARTESIAN_POINT('Ctrl Pts',(11.518694417043,1.26698486563531,0.9));
#14152=CARTESIAN_POINT('Ctrl Pts',(11.5188237574534,1.26711427133763,0.897525337604991));
#14153=CARTESIAN_POINT('Ctrl Pts',(11.5166039145442,1.26489330787379,0.939997457644392));
#14154=CARTESIAN_POINT('Ctrl Pts',(11.5143840785328,1.26267234941507,0.982469578283382));
#14155=CARTESIAN_POINT('Ctrl Pts',(11.512164249443,1.26045139597664,1.02494169952389));
#14156=CARTESIAN_POINT('Ctrl Pts',(11.560356924166,1.2626472646828,0.899468475190601));
#14157=CARTESIAN_POINT('Ctrl Pts',(11.5581357517162,1.26042470505353,0.941940442504879));
#14158=CARTESIAN_POINT('Ctrl Pts',(11.5559146107476,1.25820228015812,0.984412418590584));
#14159=CARTESIAN_POINT('Ctrl Pts',(11.5536934488601,1.25597972716877,1.02688438676053));
#14160=CARTESIAN_POINT('Ctrl Pts',(11.6290545561482,1.22266466287338,0.9009785794625));
#14161=CARTESIAN_POINT('Ctrl Pts',(11.6268300646776,1.22044146949289,0.943450343593379));
#14162=CARTESIAN_POINT('Ctrl Pts',(11.6246055668724,1.21821824717544,0.985922105839347));
#14163=CARTESIAN_POINT('Ctrl Pts',(11.6223810783988,1.21599505938238,1.02839387038768));
#14164=CARTESIAN_POINT('Ctrl Pts',(11.652916631058,1.14949843694546,0.898404198500408));
#14165=CARTESIAN_POINT('Ctrl Pts',(11.6506907663731,1.14727726203421,0.940876003223652));
#14166=CARTESIAN_POINT('Ctrl Pts',(11.6484649368037,1.14505607393729,0.9833478090785));
#14167=CARTESIAN_POINT('Ctrl Pts',(11.6462390720682,1.14283490928962,1.02581961432614));
#14168=CARTESIAN_POINT('Ctrl Pts',(11.6530022067803,1.11817769023529,0.896771316447588));
#14169=CARTESIAN_POINT('Ctrl Pts',(11.6507763512808,1.11595737261641,0.939243169479033));
#14170=CARTESIAN_POINT('Ctrl Pts',(11.6485504957647,1.11373706111287,0.981715022829298));
#14171=CARTESIAN_POINT('Ctrl Pts',(11.6463246402318,1.11151675574496,1.02418687649944));
#14172=CARTESIAN_POINT('',(11.6528329986453,1.11800890309831,0.9));
#14173=CARTESIAN_POINT('Ctrl Pts',(11.6463246402318,1.11151675574496,1.02418687649944));
#14174=CARTESIAN_POINT('Ctrl Pts',(11.6484940930522,1.11368079904038,0.982791250696082));
#14175=CARTESIAN_POINT('Ctrl Pts',(11.6506635458567,1.11584484816443,0.941395625196594));
#14176=CARTESIAN_POINT('Ctrl Pts',(11.6528329986453,1.11800890309831,0.9));
#14177=CARTESIAN_POINT('Ctrl Pts',(11.6528329986453,1.11800890309831,0.9));
#14178=CARTESIAN_POINT('Ctrl Pts',(11.6528329983633,1.12876627611802,0.899999999993021));
#14179=CARTESIAN_POINT('Ctrl Pts',(11.6516446702457,1.13947128553817,0.899998527904116));
#14180=CARTESIAN_POINT('Ctrl Pts',(11.6493511293179,1.14994150848088,0.899998119066462));
#14181=CARTESIAN_POINT('Ctrl Pts',(11.6474764306251,1.15849967852608,0.89999778488999));
#14182=CARTESIAN_POINT('Ctrl Pts',(11.6448621032167,1.16690170462481,0.899998134702192));
#14183=CARTESIAN_POINT('Ctrl Pts',(11.6415284502961,1.17504213011111,0.899998933310541));
#14184=CARTESIAN_POINT('Ctrl Pts',(11.6374537398456,1.18499213918264,0.899999909446287));
#14185=CARTESIAN_POINT('Ctrl Pts',(11.6323486952005,1.19444663470912,0.900001674548864));
#14186=CARTESIAN_POINT('Ctrl Pts',(11.6262733681268,1.20322237541324,0.900000560254235));
#14187=CARTESIAN_POINT('Ctrl Pts',(11.6256011619285,1.20419336960417,0.900000436962806));
#14188=CARTESIAN_POINT('Ctrl Pts',(11.6249170295004,1.20515603220147,0.900000274771288));
#14189=CARTESIAN_POINT('Ctrl Pts',(11.6242210175348,1.20611009565643,0.900000065883751));
#14190=CARTESIAN_POINT('Ctrl Pts',(11.6197944794931,1.21217780481426,0.899998737388448));
#14191=CARTESIAN_POINT('Ctrl Pts',(11.6148881172219,1.21789846943619,0.899995595976687));
#14192=CARTESIAN_POINT('Ctrl Pts',(11.6095544776251,1.22323873890669,0.899992615091414));
#14193=CARTESIAN_POINT('Ctrl Pts',(11.601940589012,1.23086209181126,0.899988359811689));
#14194=CARTESIAN_POINT('Ctrl Pts',(11.5935341028624,1.23763544449334,0.899984652834703));
#14195=CARTESIAN_POINT('Ctrl Pts',(11.584505756877,1.24347857204465,0.899983891616646));
#14196=CARTESIAN_POINT('Ctrl Pts',(11.5791642013329,1.24693561616068,0.899983441247493));
#14197=CARTESIAN_POINT('Ctrl Pts',(11.5736041411459,1.25006639925598,0.89998394495257));
#14198=CARTESIAN_POINT('Ctrl Pts',(11.5678562300951,1.25284717822614,0.899985279956182));
#14199=CARTESIAN_POINT('Ctrl Pts',(11.5582100984591,1.25751387535486,0.899987520356298));
#14200=CARTESIAN_POINT('Ctrl Pts',(11.548125859505,1.26115381593413,0.899992245475585));
#14201=CARTESIAN_POINT('Ctrl Pts',(11.5377575652696,1.26367454383615,0.899995957332528));
#14202=CARTESIAN_POINT('Ctrl Pts',(11.5314967650479,1.26519666246525,0.899998198703601));
#14203=CARTESIAN_POINT('Ctrl Pts',(11.5251318445822,1.26630988651457,0.89999999997641));
#14204=CARTESIAN_POINT('Ctrl Pts',(11.518694417043,1.26698486563531,0.900000000000001));
#14205=CARTESIAN_POINT('Origin',(6.0828528088686,0.,1.1));
#14206=CARTESIAN_POINT('Origin',(11.6528329986453,1.25283299864526,0.9));
#14207=CARTESIAN_POINT('',(11.6528329986453,-1.11800890309831,0.9));
#14208=CARTESIAN_POINT('Ctrl Pts',(11.6528329986453,-1.11800890309831,0.9));
#14209=CARTESIAN_POINT('Ctrl Pts',(11.6506635458567,-1.11584484816443,0.941395625196595));
#14210=CARTESIAN_POINT('Ctrl Pts',(11.6484940930522,-1.11368079904038,0.98279125069608));
#14211=CARTESIAN_POINT('Ctrl Pts',(11.6463246402318,-1.11151675574497,1.02418687649944));
#14212=CARTESIAN_POINT('',(11.6528329986453,1.25283299864526,0.9));
#14213=CARTESIAN_POINT('Ctrl Pts',(0.466487690105381,-1.07794473197144,
0.898171596006697));
#14214=CARTESIAN_POINT('Ctrl Pts',(0.468702129741454,-1.07572646385346,
0.940639831040774));
#14215=CARTESIAN_POINT('Ctrl Pts',(0.470916557169473,-1.07350820180247,
0.983108066997194));
#14216=CARTESIAN_POINT('Ctrl Pts',(0.473130972350001,-1.07128994583173,
1.02557630387858));
#14217=CARTESIAN_POINT('Ctrl Pts',(0.428364464143914,-1.0699650947497,0.899753180570758));
#14218=CARTESIAN_POINT('Ctrl Pts',(0.430581658228805,-1.06774429850715,
0.942221140547455));
#14219=CARTESIAN_POINT('Ctrl Pts',(0.432798785432897,-1.06552370176641,
0.98468911452651));
#14220=CARTESIAN_POINT('Ctrl Pts',(0.435015961689253,-1.0633029131784,1.02715707577488));
#14221=CARTESIAN_POINT('Ctrl Pts',(0.367703220512368,-1.02873213740117,
0.900780809445176));
#14222=CARTESIAN_POINT('Ctrl Pts',(0.369926480243704,-1.02651076835199,
0.943248428164859));
#14223=CARTESIAN_POINT('Ctrl Pts',(0.372149767842394,-1.02428934262989,
0.985716042409561));
#14224=CARTESIAN_POINT('Ctrl Pts',(0.374373022752712,-1.02206798136513,
1.0281836617465));
#14225=CARTESIAN_POINT('Ctrl Pts',(0.347078053061478,-0.96052525347768,
0.898302765458188));
#14226=CARTESIAN_POINT('Ctrl Pts',(0.349303707759805,-0.958307704298137,
0.940770468670701));
#14227=CARTESIAN_POINT('Ctrl Pts',(0.351529312469145,-0.956090135383351,
0.983238173449507));
#14228=CARTESIAN_POINT('Ctrl Pts',(0.35375496723721,-0.953872602525604,
1.02570587749755));
#14229=CARTESIAN_POINT('Ctrl Pts',(0.346998431491642,-0.931328747842296,
0.896783495400846));
#14230=CARTESIAN_POINT('Ctrl Pts',(0.349224074223285,-0.929112823219098,
0.939251288581378));
#14231=CARTESIAN_POINT('Ctrl Pts',(0.3514497169821,-0.926896908559584,0.98171908228038));
#14232=CARTESIAN_POINT('Ctrl Pts',(0.35367535976817,-0.924681003894255,
1.02418687649944));
#14233=CARTESIAN_POINT('',(0.466583029361856,-1.07784922788182,0.9));
#14234=CARTESIAN_POINT('Ctrl Pts',(0.347167001354737,-0.931160914046453,
0.9));
#14235=CARTESIAN_POINT('Ctrl Pts',(0.34716700178392,-0.941918922633709,
0.89999999999014));
#14236=CARTESIAN_POINT('Ctrl Pts',(0.348348457226296,-0.952625037179515,
0.899998920330619));
#14237=CARTESIAN_POINT('Ctrl Pts',(0.350635026118381,-0.963095666025449,
0.899998881610567));
#14238=CARTESIAN_POINT('Ctrl Pts',(0.352503737518513,-0.971652846855939,
0.899998849966385));
#14239=CARTESIAN_POINT('Ctrl Pts',(0.355111758040853,-0.980053468583104,
0.899999488623984));
#14240=CARTESIAN_POINT('Ctrl Pts',(0.358442500181925,-0.988191468018609,
0.900000335306729));
#14241=CARTESIAN_POINT('Ctrl Pts',(0.362154764014137,-0.997261639077022,
0.900001278973215));
#14242=CARTESIAN_POINT('Ctrl Pts',(0.366728534310471,-1.00591832418384,
0.900002536038328));
#14243=CARTESIAN_POINT('Ctrl Pts',(0.372121756320194,-1.01402249383533,
0.900001139180886));
#14244=CARTESIAN_POINT('Ctrl Pts',(0.377460617198322,-1.02204497728291,
0.899999756403108));
#14245=CARTESIAN_POINT('Ctrl Pts',(0.383603173789776,-1.02952688289601,
0.899995781932517));
#14246=CARTESIAN_POINT('Ctrl Pts',(0.390441954151244,-1.03639066990207,
0.899992822880961));
#14247=CARTESIAN_POINT('Ctrl Pts',(0.398043576670582,-1.0440200884702,0.899989533757499));
#14248=CARTESIAN_POINT('Ctrl Pts',(0.406433719974705,-1.0508151602132,0.89998759991803));
#14249=CARTESIAN_POINT('Ctrl Pts',(0.415453314813275,-1.05667842789903,
0.899988256654353));
#14250=CARTESIAN_POINT('Ctrl Pts',(0.418717986328798,-1.05880065659603,
0.899988494362188));
#14251=CARTESIAN_POINT('Ctrl Pts',(0.422065457324696,-1.0608004431648,0.89998903479261));
#14252=CARTESIAN_POINT('Ctrl Pts',(0.425489105966494,-1.06267176343868,
0.899989815051126));
#14253=CARTESIAN_POINT('Ctrl Pts',(0.434878177994434,-1.06780370385578,
0.899991954845297));
#14254=CARTESIAN_POINT('Ctrl Pts',(0.444763746614507,-1.07193185662919,
0.899996125260102));
#14255=CARTESIAN_POINT('Ctrl Pts',(0.455000483828058,-1.07494865668414,
0.899998508040168));
#14256=CARTESIAN_POINT('Ctrl Pts',(0.458814676066972,-1.07607271165555,
0.899999395860286));
#14257=CARTESIAN_POINT('Ctrl Pts',(0.462677844602733,-1.07704202188211,
0.899999999981245));
#14258=CARTESIAN_POINT('Ctrl Pts',(0.466583029361856,-1.07784922788182,
0.9));
#14259=CARTESIAN_POINT('Ctrl Pts',(0.466583029361855,-1.07784922788182,
0.9));
#14260=CARTESIAN_POINT('Ctrl Pts',(0.468754418912838,-1.07567408410356,
0.941642632722455));
#14261=CARTESIAN_POINT('Ctrl Pts',(0.470925796725269,-1.07349894615889,
0.983285266331777));
#14262=CARTESIAN_POINT('Ctrl Pts',(0.473097162761967,-1.07132381406029,
1.02492790083044));
#14263=CARTESIAN_POINT('Ctrl Pts',(11.6530064742455,-1.11818194708322,0.896689888359234));
#14264=CARTESIAN_POINT('Ctrl Pts',(11.6507791962577,-1.11596021050721,0.93918888408639));
#14265=CARTESIAN_POINT('Ctrl Pts',(11.6485519182532,-1.11373848005435,0.98168788013277));
#14266=CARTESIAN_POINT('Ctrl Pts',(11.6463246402318,-1.11151675574497,1.02418687649944));
#14267=CARTESIAN_POINT('Ctrl Pts',(11.6528923732761,-1.15994294490385,0.898867064552409));
#14268=CARTESIAN_POINT('Ctrl Pts',(11.6506650597175,-1.15772003758575,0.94136599317676));
#14269=CARTESIAN_POINT('Ctrl Pts',(11.6484378630123,-1.15549719156343,0.98386493116262));
#14270=CARTESIAN_POINT('Ctrl Pts',(11.646210549347,-1.15327429380451,1.02636386026838));
#14271=CARTESIAN_POINT('Ctrl Pts',(11.6202781937939,-1.23241532269502,0.900946494593638));
#14272=CARTESIAN_POINT('Ctrl Pts',(11.6180528194216,-1.23019050716461,0.943445418126786));
#14273=CARTESIAN_POINT('Ctrl Pts',(11.61582741935,-1.22796567893144,0.985944339620759));
#14274=CARTESIAN_POINT('Ctrl Pts',(11.6136020491686,-1.22574086850162,1.02844326360542));
#14275=CARTESIAN_POINT('Ctrl Pts',(11.5499778903249,-1.26376827666489,0.89890126240954));
#14276=CARTESIAN_POINT('Ctrl Pts',(11.5477556460229,-1.26154471817669,0.941400412665532));
#14277=CARTESIAN_POINT('Ctrl Pts',(11.5455333818837,-1.25932119531825,0.983899563748029));
#14278=CARTESIAN_POINT('Ctrl Pts',(11.5433111490058,-1.25709764437074,1.02639871495137));
#14279=CARTESIAN_POINT('Ctrl Pts',(11.5188280133912,-1.26711852942379,0.897443909004722));
#14280=CARTESIAN_POINT('Ctrl Pts',(11.5166067518272,-1.2648961465915,0.93994317191011));
#14281=CARTESIAN_POINT('Ctrl Pts',(11.5143854971699,-1.26267376877071,0.982442435415857));
#14282=CARTESIAN_POINT('Ctrl Pts',(11.512164249443,-1.26045139597664,1.02494169952389));
#14283=CARTESIAN_POINT('',(11.518694417043,-1.26698486563531,0.9));
#14284=CARTESIAN_POINT('Ctrl Pts',(11.5121826600865,-1.26046981594517,1.02458944759559));
#14285=CARTESIAN_POINT('Ctrl Pts',(11.5143532391283,-1.26264149437998,0.983059631155874));
#14286=CARTESIAN_POINT('Ctrl Pts',(11.5165238247878,-1.26481317761477,0.941529815291278));
#14287=CARTESIAN_POINT('Ctrl Pts',(11.518694417043,-1.26698486563531,0.900000000000001));
#14288=CARTESIAN_POINT('Ctrl Pts',(11.518694417043,-1.26698486563531,0.9));
#14289=CARTESIAN_POINT('Ctrl Pts',(11.5293907449245,-1.26586333143554,0.89999999999772));
#14290=CARTESIAN_POINT('Ctrl Pts',(11.5399108669542,-1.26356499290392,0.899998338215302));
#14291=CARTESIAN_POINT('Ctrl Pts',(11.5500820708623,-1.26019169516113,0.899997799246518));
#14292=CARTESIAN_POINT('Ctrl Pts',(11.5583854467913,-1.257437865867,0.899997359253331));
#14293=CARTESIAN_POINT('Ctrl Pts',(11.5664568733073,-1.25396634382171,0.899997630752438));
#14294=CARTESIAN_POINT('Ctrl Pts',(11.5741940388996,-1.24980829733595,0.899998424072895));
#14295=CARTESIAN_POINT('Ctrl Pts',(11.5836658766397,-1.2447180170313,0.899999395255759));
#14296=CARTESIAN_POINT('Ctrl Pts',(11.5925370694996,-1.23865400393036,0.900001263097414));
#14297=CARTESIAN_POINT('Ctrl Pts',(11.6006317325417,-1.23169548876955,0.900000312360774));
#14298=CARTESIAN_POINT('Ctrl Pts',(11.6015335603822,-1.23092023936527,0.900000206439036));
#14299=CARTESIAN_POINT('Ctrl Pts',(11.602425722662,-1.23013384139825,0.900000061718141));
#14300=CARTESIAN_POINT('Ctrl Pts',(11.6033079529217,-1.22933637123764,0.899999870107331));
#14301=CARTESIAN_POINT('Ctrl Pts',(11.6088666967428,-1.22431168263841,0.899998662808674));
#14302=CARTESIAN_POINT('Ctrl Pts',(11.6140319692072,-1.21884801843051,0.89999566823453));
#14303=CARTESIAN_POINT('Ctrl Pts',(11.6187763833168,-1.21300082485405,0.899992820294732));
#14304=CARTESIAN_POINT('Ctrl Pts',(11.6255647330688,-1.20463460846846,0.899988745437233));
#14305=CARTESIAN_POINT('Ctrl Pts',(11.6314252437734,-1.1955686993246,0.899985180772245));
#14306=CARTESIAN_POINT('Ctrl Pts',(11.6362963259193,-1.18598144606113,0.899984461491908));
#14307=CARTESIAN_POINT('Ctrl Pts',(11.6391835002004,-1.18029891593343,0.899984035162064));
#14308=CARTESIAN_POINT('Ctrl Pts',(11.6417223485433,-1.1744324689719,0.89998453059116));
#14309=CARTESIAN_POINT('Ctrl Pts',(11.6438924319112,-1.16841525789854,0.899985826675912));
#14310=CARTESIAN_POINT('Ctrl Pts',(11.6475288754212,-1.15833212078062,0.899987998545922));
#14311=CARTESIAN_POINT('Ctrl Pts',(11.650098554646,-1.1479202064002,0.899992549671115));
#14312=CARTESIAN_POINT('Ctrl Pts',(11.6515257507029,-1.13734249630077,0.899996116295739));
#14313=CARTESIAN_POINT('Ctrl Pts',(11.6523885972688,-1.13094748084967,0.899998272586596));
#14314=CARTESIAN_POINT('Ctrl Pts',(11.6528329982118,-1.12449140232308,0.899999999966183));
#14315=CARTESIAN_POINT('Ctrl Pts',(11.6528329986453,-1.11800890309831,0.9));
#14316=CARTESIAN_POINT('Origin',(6.08275255467124,0.,0.9));
#14317=CARTESIAN_POINT('Ctrl Pts',(11.518694417043,-1.26698486563531,0.9));
#14318=CARTESIAN_POINT('Ctrl Pts',(7.83465728781595,-1.65326443611903,0.9));
#14319=CARTESIAN_POINT('Ctrl Pts',(4.1506201585889,-1.83934349355009,0.9));
#14320=CARTESIAN_POINT('Ctrl Pts',(0.466583029361856,-1.07784922788182,
0.9));
#14321=CARTESIAN_POINT('Ctrl Pts',(11.518694417043,-1.26698486563531,0.9));
#14322=CARTESIAN_POINT('Ctrl Pts',(11.516563806181,-1.26480246768431,0.941642633610146));
#14323=CARTESIAN_POINT('Ctrl Pts',(11.514433195319,-1.2626200697333,0.983285267220291));
#14324=CARTESIAN_POINT('Ctrl Pts',(11.512302584457,-1.2604376717823,1.02492790083044));
#14325=CARTESIAN_POINT('Ctrl Pts',(7.83465728781595,-1.65326443611903,0.9));
#14326=CARTESIAN_POINT('Ctrl Pts',(7.83394897884827,-1.65108203816803,0.941642633610146));
#14327=CARTESIAN_POINT('Ctrl Pts',(7.83324066988059,-1.64889964021702,0.983285267220291));
#14328=CARTESIAN_POINT('Ctrl Pts',(7.83253236091292,-1.64671724226602,1.02492790083044));
#14329=CARTESIAN_POINT('Ctrl Pts',(4.1506201585889,-1.8393434935501,0.9));
#14330=CARTESIAN_POINT('Ctrl Pts',(4.15133415151555,-1.83716109559909,0.941642633610146));
#14331=CARTESIAN_POINT('Ctrl Pts',(4.15204814444219,-1.83497869764808,0.983285267220291));
#14332=CARTESIAN_POINT('Ctrl Pts',(4.15276213736883,-1.83279629969708,1.02492790083044));
#14333=CARTESIAN_POINT('Ctrl Pts',(0.466583029361856,-1.07784922788182,
0.9));
#14334=CARTESIAN_POINT('Ctrl Pts',(0.468719324182819,-1.07566682993082,
0.941642633610146));
#14335=CARTESIAN_POINT('Ctrl Pts',(0.470855619003783,-1.07348443197981,
0.983285267220291));
#14336=CARTESIAN_POINT('Ctrl Pts',(0.472991913824746,-1.07130203402881,
1.02492790083044));
#14337=CARTESIAN_POINT('',(0.,0.,0.));
#14338=CARTESIAN_POINT('Origin',(0.,0.,0.));
#14339=CARTESIAN_POINT('',(-0.14652705620645,9.44412402177196E-5,0.0160655045842905));
#14340=CARTESIAN_POINT('',(-0.146479946776166,0.000162062070299865,0.00893449541571059));
#14341=CARTESIAN_POINT('',(-0.14635,-1.79227059055215E-17,0.));
#14342=CARTESIAN_POINT('',(0.0634007094575209,0.131904027763685,0.));
#14343=CARTESIAN_POINT('Ctrl Pts',(-0.14652705620645,9.44412402177196E-5,
0.0160655045842905));
#14344=CARTESIAN_POINT('Ctrl Pts',(-0.146560923555419,0.00502618404349199,
0.0157963945919035));
#14345=CARTESIAN_POINT('Ctrl Pts',(-0.146333578783787,0.00995455679532004,
0.0155272845995164));
#14346=CARTESIAN_POINT('Ctrl Pts',(-0.14583475180505,0.0148550342388422,
0.0152581746071293));
#14347=CARTESIAN_POINT('Ctrl Pts',(-0.140929468554047,0.0630445487404258,
0.0126118447280274));
#14348=CARTESIAN_POINT('Ctrl Pts',(-0.10977174472993,0.108536575508351,
0.0099655148489255));
#14349=CARTESIAN_POINT('Ctrl Pts',(-0.0666135938566871,0.13056551637767,
0.00731918496982359));
#14350=CARTESIAN_POINT('Ctrl Pts',(-0.0268248419338395,0.150874636338504,
0.00487945664654906));
#14351=CARTESIAN_POINT('Ctrl Pts',(0.0231637104697219,0.151241233100125,
0.00243972832327453));
#14352=CARTESIAN_POINT('Ctrl Pts',(0.0635546915223951,0.132092229195826,
-2.16840434497101E-19));
#14353=CARTESIAN_POINT('',(-0.0634007094575146,0.131904027763688,0.));
#14354=CARTESIAN_POINT('Origin',(0.,0.,0.));
#14355=CARTESIAN_POINT('Ctrl Pts',(-0.0634007094575145,0.131904027763688,
-3.88578058618805E-16));
#14356=CARTESIAN_POINT('Ctrl Pts',(-0.107282641710421,0.110811831533068,
0.00264738937425961));
#14357=CARTESIAN_POINT('Ctrl Pts',(-0.139432201149969,0.0662847592091173,
0.00529477874851962));
#14358=CARTESIAN_POINT('Ctrl Pts',(-0.145436119191498,0.0182745223106641,
0.00794216812277962));
#14359=CARTESIAN_POINT('Ctrl Pts',(-0.146186273512714,0.0122759249909008,
0.00827294388708994));
#14360=CARTESIAN_POINT('Ctrl Pts',(-0.146528267289359,0.00622295186417552,
0.00860371965140026));
#14361=CARTESIAN_POINT('Ctrl Pts',(-0.146479946776166,0.000162062070299865,
0.00893449541571059));
#14362=CARTESIAN_POINT('Origin',(0.,0.,0.));
#14363=CARTESIAN_POINT('',(-0.146148830924315,7.59978318484386E-5,0.0660655045842905));
#14364=CARTESIAN_POINT('',(-0.146133770585873,6.2751561688711E-5,0.0589344954157103));
#14365=CARTESIAN_POINT('',(-0.14635,-1.79227059055215E-17,0.));
#14366=CARTESIAN_POINT('Ctrl Pts',(-0.146148830924315,7.59978318484386E-5,
0.0660655045842905));
#14367=CARTESIAN_POINT('Ctrl Pts',(-0.146240443598182,0.0195917497831913,
0.0650077071998482));
#14368=CARTESIAN_POINT('Ctrl Pts',(-0.142607114239671,0.0390747476468127,
0.0639499098154059));
#14369=CARTESIAN_POINT('Ctrl Pts',(-0.135087779856993,0.056920264102034,
0.0628921124309636));
#14370=CARTESIAN_POINT('Ctrl Pts',(-0.116276389754784,0.10156503643559,
0.0602457825518617));
#14371=CARTESIAN_POINT('Ctrl Pts',(-0.073143724514267,0.135961331060063,
0.0575994526727599));
#14372=CARTESIAN_POINT('Ctrl Pts',(-0.025432083612881,0.144366623974243,
0.054953122793658));
#14373=CARTESIAN_POINT('Ctrl Pts',(0.0222795572885053,0.152771916888423,
0.0523067929145561));
#14374=CARTESIAN_POINT('Ctrl Pts',(0.0745701738507606,0.135186208092309,
0.0496604630354541));
#14375=CARTESIAN_POINT('Ctrl Pts',(0.107505148494886,0.0996564726649905,
0.0470141331563522));
#14376=CARTESIAN_POINT('Ctrl Pts',(0.140440123139012,0.0641267372376721,
0.0443678032772503));
#14377=CARTESIAN_POINT('Ctrl Pts',(0.154019455865009,0.010652975179149,
0.0417214733981484));
#14378=CARTESIAN_POINT('Ctrl Pts',(0.14202839331759,-0.0362847016460775,
0.0390751435190465));
#14379=CARTESIAN_POINT('Ctrl Pts',(0.130037330770172,-0.0832223784713041,
0.0364288136399446));
#14380=CARTESIAN_POINT('Ctrl Pts',(0.0924758729493388,-0.123623970063234,
0.0337824837608427));
#14381=CARTESIAN_POINT('Ctrl Pts',(0.0465351214488668,-0.139005253038876,
0.0311361538817407));
#14382=CARTESIAN_POINT('Ctrl Pts',(0.000594369948394902,-0.154386536014517,
0.0284898240026388));
#14383=CARTESIAN_POINT('Ctrl Pts',(-0.0537256752317158,-0.144747510373871,
0.025843494123537));
#14384=CARTESIAN_POINT('Ctrl Pts',(-0.0915592764828275,-0.114484496435928,
0.0231971642444351));
#14385=CARTESIAN_POINT('Ctrl Pts',(-0.125545511528741,-0.0872989822136326,
0.0208199443577202));
#14386=CARTESIAN_POINT('Ctrl Pts',(-0.146227884351973,-0.0434707826450544,
0.0184427244710054));
#14387=CARTESIAN_POINT('Ctrl Pts',(-0.14652705620645,9.44412402177196E-5,
0.0160655045842905));
#14388=CARTESIAN_POINT('Ctrl Pts',(-0.146479946776166,0.000162062070299865,
0.00893449541571059));
#14389=CARTESIAN_POINT('Ctrl Pts',(-0.146141530330399,-0.0422858476614564,
0.0112511090256603));
#14390=CARTESIAN_POINT('Ctrl Pts',(-0.126658161292025,-0.0851220706608281,
0.0135677226356099));
#14391=CARTESIAN_POINT('Ctrl Pts',(-0.0941604943243988,-0.112386678841155,
0.0158843362455596));
#14392=CARTESIAN_POINT('Ctrl Pts',(-0.0570226747722624,-0.143544241621566,
0.0185317256198196));
#14393=CARTESIAN_POINT('Ctrl Pts',(-0.00288875902448078,-0.154365965709432,
0.0211791149940796));
#14394=CARTESIAN_POINT('Ctrl Pts',(0.0434083729543798,-0.140002007265973,
0.0238265043683396));
#14395=CARTESIAN_POINT('Ctrl Pts',(0.0897055049332404,-0.125638048822514,
0.0264738937425996));
#14396=CARTESIAN_POINT('Ctrl Pts',(0.12816585314318,-0.0860884078477292,
0.0291212831168596));
#14397=CARTESIAN_POINT('Ctrl Pts',(0.141191617966992,-0.0394144013492358,
0.0317686724911196));
#14398=CARTESIAN_POINT('Ctrl Pts',(0.154217382790803,0.00725960514925768,
0.0344160618653796));
#14399=CARTESIAN_POINT('Ctrl Pts',(0.141808564228487,0.0610579771714599,
0.0370634512396396));
#14400=CARTESIAN_POINT('Ctrl Pts',(0.109639063769471,0.0973098477439542,
0.0397108406138996));
#14401=CARTESIAN_POINT('Ctrl Pts',(0.0774695633104545,0.133561718316448,
0.0423582299881596));
#14402=CARTESIAN_POINT('Ctrl Pts',(0.0255393809547383,0.152267087439235,
0.0450056193624196));
#14403=CARTESIAN_POINT('Ctrl Pts',(-0.0223595433272462,0.144872892294413,
0.0476530087366796));
#14404=CARTESIAN_POINT('Ctrl Pts',(-0.070258467609231,0.137478697149591,
0.0503003981109396));
#14405=CARTESIAN_POINT('Ctrl Pts',(-0.114126133817484,0.10398493773716,
0.0529477874851996));
#14406=CARTESIAN_POINT('Ctrl Pts',(-0.133871661545403,0.059725601630819,
0.0555951768594596));
#14407=CARTESIAN_POINT('Ctrl Pts',(-0.142173753131161,0.0411165744656389,
0.0567082830448765));
#14408=CARTESIAN_POINT('Ctrl Pts',(-0.146211489678532,0.0206043892842972,
0.0578213892302934));
#14409=CARTESIAN_POINT('Ctrl Pts',(-0.146133770585873,6.2751561688711E-5,
0.0589344954157103));
#14410=CARTESIAN_POINT('Origin',(0.,0.,0.));
#14411=CARTESIAN_POINT('',(-0.146252097264499,-0.000124487410312429,0.116065504584291));
#14412=CARTESIAN_POINT('',(-0.146276374479508,-0.000129480650117819,0.10893449541571));
#14413=CARTESIAN_POINT('',(-0.14635,-1.79227059055215E-17,0.));
#14414=CARTESIAN_POINT('Ctrl Pts',(-0.146252097264499,-0.000124487410312429,
0.116065504584291));
#14415=CARTESIAN_POINT('Ctrl Pts',(-0.145977101830714,0.0338815411246725,
0.114219019807793));
#14416=CARTESIAN_POINT('Ctrl Pts',(-0.134160879762789,0.0680598926014691,
0.112372535031295));
#14417=CARTESIAN_POINT('Ctrl Pts',(-0.112484833627769,0.0939988017516943,
0.110526050254798));
#14418=CARTESIAN_POINT('Ctrl Pts',(-0.0814193359437304,0.131173714423195,
0.107879720375696));
#14419=CARTESIAN_POINT('Ctrl Pts',(-0.0301019434218634,0.151424966146533,
0.105233390496594));
#14420=CARTESIAN_POINT('Ctrl Pts',(0.0179785702873004,0.145483266051774,
0.102587060617492));
#14421=CARTESIAN_POINT('Ctrl Pts',(0.0660590839964643,0.139541565957016,
0.0999407307383904));
#14422=CARTESIAN_POINT('Ctrl Pts',(0.110902718892925,0.107406914044162,
0.0972944008592884));
#14423=CARTESIAN_POINT('Ctrl Pts',(0.131983829661647,0.0637877973597534,
0.0946480709801865));
#14424=CARTESIAN_POINT('Ctrl Pts',(0.15306494043037,0.0201686806753445,
0.0920017411010846));
#14425=CARTESIAN_POINT('Ctrl Pts',(0.150383527071356,-0.0349349007806195,
0.0893554112219828));
#14426=CARTESIAN_POINT('Ctrl Pts',(0.125166930059577,-0.0763010783846813,
0.0867090813428809));
#14427=CARTESIAN_POINT('Ctrl Pts',(0.0999503330477985,-0.117667255988743,
0.084062751463779));
#14428=CARTESIAN_POINT('Ctrl Pts',(0.0521985523832557,-0.145296029740903,
0.081416421584677));
#14429=CARTESIAN_POINT('Ctrl Pts',(0.00376830011669856,-0.146541450754272,
0.0787700917055751));
#14430=CARTESIAN_POINT('Ctrl Pts',(-0.0446619521498586,-0.147786871767642,
0.0761237618264732));
#14431=CARTESIAN_POINT('Ctrl Pts',(-0.09377067601843,-0.122648940042221,
0.0734774319473713));
#14432=CARTESIAN_POINT('Ctrl Pts',(-0.121079980470766,-0.0826333491581908,
0.0708311020682694));
#14433=CARTESIAN_POINT('Ctrl Pts',(-0.137473143648068,-0.0586128871159229,
0.0692425695736098));
#14434=CARTESIAN_POINT('Ctrl Pts',(-0.146011252866834,-0.02923151094855,
0.0676540370789502));
#14435=CARTESIAN_POINT('Ctrl Pts',(-0.146148830924315,7.59978318484386E-5,
0.0660655045842905));
#14436=CARTESIAN_POINT('Ctrl Pts',(-0.146133770585873,6.2751561688711E-5,
0.0589344954157103));
#14437=CARTESIAN_POINT('Ctrl Pts',(-0.146026644150963,-0.0282514289199324,
0.0604687786045534));
#14438=CARTESIAN_POINT('Ctrl Pts',(-0.138100435392092,-0.0566215672018456,
0.0620030617933965));
#14439=CARTESIAN_POINT('Ctrl Pts',(-0.122745086057252,-0.0801407530065182,
0.0635373449822396));
#14440=CARTESIAN_POINT('Ctrl Pts',(-0.0962495935935968,-0.120722858737265,
0.0661847343564996));
#14441=CARTESIAN_POINT('Ctrl Pts',(-0.0476352194187008,-0.146862157398507,
0.0688321237307596));
#14442=CARTESIAN_POINT('Ctrl Pts',(0.00082938917649622,-0.146587691816784,
0.0714795131050196));
#14443=CARTESIAN_POINT('Ctrl Pts',(0.0492939977716932,-0.146313226235061,
0.0741269024792796));
#14444=CARTESIAN_POINT('Ctrl Pts',(0.0976088407871913,-0.119624996410372,
0.0767742918535397));
#14445=CARTESIAN_POINT('Ctrl Pts',(0.123643642180798,-0.0787464320231966,
0.0794216812277997));
#14446=CARTESIAN_POINT('Ctrl Pts',(0.149678443574405,-0.0378678676360213,
0.0820690706020596));
#14447=CARTESIAN_POINT('Ctrl Pts',(0.153433203346121,0.0172010313136401,
0.0847164599763195));
#14448=CARTESIAN_POINT('Ctrl Pts',(0.133187835944515,0.06123527443138,0.0873638493505795));
#14449=CARTESIAN_POINT('Ctrl Pts',(0.11294246854291,0.10526951754912,0.0900112387248395));
#14450=CARTESIAN_POINT('Ctrl Pts',(0.0686969739679828,0.138269104834938,
0.0926586280990997));
#14451=CARTESIAN_POINT('Ctrl Pts',(0.0207181735233275,0.145118849380084,
0.0953060174733597));
#14452=CARTESIAN_POINT('Ctrl Pts',(-0.027260626921328,0.151968593925229,
0.0979534068476197));
#14453=CARTESIAN_POINT('Ctrl Pts',(-0.0789727332357116,0.132668495729702,
0.10060079622188));
#14454=CARTESIAN_POINT('Ctrl Pts',(-0.110731403441959,0.0960588230543748,
0.10324818559614));
#14455=CARTESIAN_POINT('Ctrl Pts',(-0.133469481440122,0.0698475998711364,
0.105143622202663));
#14456=CARTESIAN_POINT('Ctrl Pts',(-0.145979327216774,0.0347634013028336,
0.107039058809187));
#14457=CARTESIAN_POINT('Ctrl Pts',(-0.146276374479508,-0.000129480650117819,
0.10893449541571));
#14458=CARTESIAN_POINT('Origin',(0.,0.,0.));
#14459=CARTESIAN_POINT('',(-0.146589818999335,-3.81787486967988E-6,0.166065504584291));
#14460=CARTESIAN_POINT('',(-0.146589453522336,1.04004190909306E-5,0.15893449541571));
#14461=CARTESIAN_POINT('',(-0.14635,-1.79227059055215E-17,0.));
#14462=CARTESIAN_POINT('Ctrl Pts',(-0.146589818999335,-3.81787486967988E-6,
0.166065504584291));
#14463=CARTESIAN_POINT('Ctrl Pts',(-0.146571339149733,0.0482382848470949,
0.163430332415738));
#14464=CARTESIAN_POINT('Ctrl Pts',(-0.120433071521034,0.0964975486977609,
0.160795160247185));
#14465=CARTESIAN_POINT('Ctrl Pts',(-0.0800107885095625,0.122828684230981,
0.158159988078632));
#14466=CARTESIAN_POINT('Ctrl Pts',(-0.0394173515450545,0.149271309704865,
0.15551365819953));
#14467=CARTESIAN_POINT('Ctrl Pts',(0.0155813181737399,0.153599719825856,
0.152867328320428));
#14468=CARTESIAN_POINT('Ctrl Pts',(0.0598114643267532,0.133832733731537,
0.150220998441327));
#14469=CARTESIAN_POINT('Ctrl Pts',(0.104041610479766,0.114065747637217,
0.147574668562225));
#14470=CARTESIAN_POINT('Ctrl Pts',(0.137503233066998,0.0702033653275883,
0.144928338683123));
#14471=CARTESIAN_POINT('Ctrl Pts',(0.144880420813362,0.0223220882221681,
0.142282008804021));
#14472=CARTESIAN_POINT('Ctrl Pts',(0.152257608559726,-0.0255591888832524,
0.139635678924919));
#14473=CARTESIAN_POINT('Ctrl Pts',(0.133550361465222,-0.077459360784464,
0.136989349045817));
#14474=CARTESIAN_POINT('Ctrl Pts',(0.0973212811704284,-0.109622900294719,
0.134343019166715));
#14475=CARTESIAN_POINT('Ctrl Pts',(0.0610922008756344,-0.141786439804975,
0.131696689287613));
#14476=CARTESIAN_POINT('Ctrl Pts',(0.00734128738055008,-0.154213346924274,
0.129050359408511));
#14477=CARTESIAN_POINT('Ctrl Pts',(-0.0393288211819405,-0.141215634503184,
0.126404029529409));
#14478=CARTESIAN_POINT('Ctrl Pts',(-0.0859989297444312,-0.128217922082094,
0.123757699650308));
#14479=CARTESIAN_POINT('Ctrl Pts',(-0.125588233374328,-0.0897955901206149,
0.121111369771206));
#14480=CARTESIAN_POINT('Ctrl Pts',(-0.139976083766172,-0.043535137330043,
0.118465039892104));
#14481=CARTESIAN_POINT('Ctrl Pts',(-0.144324767489921,-0.0295530571287048,
0.117665194789499));
#14482=CARTESIAN_POINT('Ctrl Pts',(-0.146371217526823,-0.0148549394177889,
0.116865349686895));
#14483=CARTESIAN_POINT('Ctrl Pts',(-0.146252097264499,-0.000124487410312429,
0.116065504584291));
#14484=CARTESIAN_POINT('Ctrl Pts',(-0.146276374479508,-0.000129480650117819,
0.10893449541571));
#14485=CARTESIAN_POINT('Ctrl Pts',(-0.14639421831063,-0.0139720956278579,
0.109686448183447));
#14486=CARTESIAN_POINT('Ctrl Pts',(-0.14458995413065,-0.0277846002915201,
0.110438400951183));
#14487=CARTESIAN_POINT('Ctrl Pts',(-0.140739671041232,-0.041001045008257,
0.11119035371892));
#14488=CARTESIAN_POINT('Ctrl Pts',(-0.127184034336146,-0.0875319932404337,
0.11383774309318));
#14489=CARTESIAN_POINT('Ctrl Pts',(-0.0882675268278623,-0.12667464254966,
0.11648513246744));
#14490=CARTESIAN_POINT('Ctrl Pts',(-0.0418159243469935,-0.140499695546946,
0.1191325218417));
#14491=CARTESIAN_POINT('Ctrl Pts',(0.00463567813387508,-0.154324748544231,
0.12177991121596));
#14492=CARTESIAN_POINT('Ctrl Pts',(0.0586223755873289,-0.142832205229577,
0.12442730059022));
#14493=CARTESIAN_POINT('Ctrl Pts',(0.0954154960694136,-0.111286216216264,
0.12707468996448));
#14494=CARTESIAN_POINT('Ctrl Pts',(0.132208616551499,-0.0797402272029501,
0.12972207933874));
#14495=CARTESIAN_POINT('Ctrl Pts',(0.151808160062214,-0.0281407924909768,
0.132369468712999));
#14496=CARTESIAN_POINT('Ctrl Pts',(0.145236524363737,0.0198768833792122,
0.135016858087259));
#14497=CARTESIAN_POINT('Ctrl Pts',(0.138664888665259,0.0678945592494009,
0.13766424746152));
#14498=CARTESIAN_POINT('Ctrl Pts',(0.105922073757589,0.112330476277805,
0.14031163683578));
#14499=CARTESIAN_POINT('Ctrl Pts',(0.062005973158836,0.132830708741579,
0.14295902621004));
#14500=CARTESIAN_POINT('Ctrl Pts',(0.0180898725600832,0.153330941205352,
0.1456064155843));
#14501=CARTESIAN_POINT('Ctrl Pts',(-0.0369995137297515,0.149895489104495,
0.14825380495856));
#14502=CARTESIAN_POINT('Ctrl Pts',(-0.0780284182758478,0.124097962381086,
0.15090119433282));
#14503=CARTESIAN_POINT('Ctrl Pts',(-0.119057322821944,0.0983004356576776,
0.153548583707079));
#14504=CARTESIAN_POINT('Ctrl Pts',(-0.146025745624302,0.0501408343117172,
0.15619597308134));
#14505=CARTESIAN_POINT('Ctrl Pts',(-0.14658076309025,0.00167873146180186,
0.1588433624556));
#14506=CARTESIAN_POINT('Ctrl Pts',(-0.146587131676737,0.00112264969450139,
0.15887374010897));
#14507=CARTESIAN_POINT('Ctrl Pts',(-0.146590022522527,0.000566528098114988,
0.15890411776234));
#14508=CARTESIAN_POINT('Ctrl Pts',(-0.146589453522336,1.04004190909306E-5,
0.15893449541571));
#14509=CARTESIAN_POINT('Origin',(0.,0.,0.));
#14510=CARTESIAN_POINT('',(-0.146263250741535,0.000126870157254357,0.21606550458429));
#14511=CARTESIAN_POINT('',(-0.146245769975643,0.000123264779366826,0.20893449541571));
#14512=CARTESIAN_POINT('',(-0.14635,-1.79227059055215E-17,0.));
#14513=CARTESIAN_POINT('Ctrl Pts',(-0.146263250741535,0.000126870157254357,
0.21606550458429));
#14514=CARTESIAN_POINT('Ctrl Pts',(-0.146381923100139,0.0144435832128767,
0.215287974902784));
#14515=CARTESIAN_POINT('Ctrl Pts',(-0.144450237714319,0.0287289633064517,
0.214510445221278));
#14516=CARTESIAN_POINT('Ctrl Pts',(-0.140337374518256,0.0423560295890773,
0.213732915539772));
#14517=CARTESIAN_POINT('Ctrl Pts',(-0.126339204386259,0.0887358830222778,
0.21108658566067));
#14518=CARTESIAN_POINT('Ctrl Pts',(-0.0870745347363382,0.127489909020004,
0.208440255781569));
#14519=CARTESIAN_POINT('Ctrl Pts',(-0.0405154226099946,0.140879780169064,
0.205793925902467));
#14520=CARTESIAN_POINT('Ctrl Pts',(0.00604368951634975,0.154269651318124,
0.203147596023365));
#14521=CARTESIAN_POINT('Ctrl Pts',(0.0598972441191175,0.142295367618517,
0.200501266144263));
#14522=CARTESIAN_POINT('Ctrl Pts',(0.0963956219934077,0.110437747119808,
0.197854936265161));
#14523=CARTESIAN_POINT('Ctrl Pts',(0.132893999867697,0.0785801266211,0.195208606386059));
#14524=CARTESIAN_POINT('Ctrl Pts',(0.15203720101351,0.0268391693232909,
0.192562276506957));
#14525=CARTESIAN_POINT('Ctrl Pts',(0.145063081087281,-0.0211024746124516,
0.189915946627855));
#14526=CARTESIAN_POINT('Ctrl Pts',(0.138088961161051,-0.0690441185481943,
0.187269616748753));
#14527=CARTESIAN_POINT('Ctrl Pts',(0.10499752016278,-0.11318644912187,0.184623286869651));
#14528=CARTESIAN_POINT('Ctrl Pts',(0.060935231264163,-0.133324827106958,
0.181976956990549));
#14529=CARTESIAN_POINT('Ctrl Pts',(0.0168729423655461,-0.153463205092045,
0.179330627111448));
#14530=CARTESIAN_POINT('Ctrl Pts',(-0.0381601944334158,-0.149597630488544,
0.176684297232346));
#14531=CARTESIAN_POINT('Ctrl Pts',(-0.0789746466099193,-0.123497437688695,
0.174037967353244));
#14532=CARTESIAN_POINT('Ctrl Pts',(-0.119961184605052,-0.0972871987457574,
0.171380479763593));
#14533=CARTESIAN_POINT('Ctrl Pts',(-0.146608455341797,-0.0486544490602708,
0.168722992173942));
#14534=CARTESIAN_POINT('Ctrl Pts',(-0.146589818999335,-3.81787486967988E-6,
0.166065504584291));
#14535=CARTESIAN_POINT('Ctrl Pts',(-0.146589453522336,1.04004190909306E-5,
0.15893449541571));
#14536=CARTESIAN_POINT('Ctrl Pts',(-0.146540434588914,-0.0478995759235739,
0.1615515071366));
#14537=CARTESIAN_POINT('Ctrl Pts',(-0.120813506558866,-0.0958546957256878,
0.16416851885749));
#14538=CARTESIAN_POINT('Ctrl Pts',(-0.0808500697395765,-0.122278388912248,
0.16678553057838));
#14539=CARTESIAN_POINT('Ctrl Pts',(-0.0404227467934142,-0.149008802082514,
0.16943291995264));
#14540=CARTESIAN_POINT('Ctrl Pts',(0.0145735112284506,-0.153705024069172,
0.1720803093269));
#14541=CARTESIAN_POINT('Ctrl Pts',(0.0589475933459444,-0.134215943447351,
0.17472769870116));
#14542=CARTESIAN_POINT('Ctrl Pts',(0.103321675463438,-0.11472686282553,
0.17737508807542));
#14543=CARTESIAN_POINT('Ctrl Pts',(0.137073581676561,-0.0710524795952304,
0.18002247744968));
#14544=CARTESIAN_POINT('Ctrl Pts',(0.144743205110219,-0.0231979049720499,
0.18266986682394));
#14545=CARTESIAN_POINT('Ctrl Pts',(0.152412828543877,0.024656669651131,
0.1853172561982));
#14546=CARTESIAN_POINT('Ctrl Pts',(0.13400016919807,0.0766914356671922,
0.18796464557246));
#14547=CARTESIAN_POINT('Ctrl Pts',(0.0979391709064228,0.109071797518936,
0.19061203494672));
#14548=CARTESIAN_POINT('Ctrl Pts',(0.0618781726147763,0.141452159370678,
0.19325942432098));
#14549=CARTESIAN_POINT('Ctrl Pts',(0.00816883537729064,0.154178117058104,
0.195906813695239));
#14550=CARTESIAN_POINT('Ctrl Pts',(-0.0385872054932313,0.1414205281901,
0.198554203069499));
#14551=CARTESIAN_POINT('Ctrl Pts',(-0.0853432463637543,0.128662939322095,
0.201201592443759));
#14552=CARTESIAN_POINT('Ctrl Pts',(-0.125145990867313,0.0904218038986596,
0.20384898181802));
#14553=CARTESIAN_POINT('Ctrl Pts',(-0.139763737461459,0.0442135263146365,
0.20649637119228));
#14554=CARTESIAN_POINT('Ctrl Pts',(-0.144251162244238,0.030028291356252,
0.207309079266757));
#14555=CARTESIAN_POINT('Ctrl Pts',(-0.146365162502875,0.0150922359825044,
0.208121787341234));
#14556=CARTESIAN_POINT('Ctrl Pts',(-0.146245769975643,0.000123264779366826,
0.20893449541571));
#14557=CARTESIAN_POINT('Origin',(0.,0.,0.));
#14558=CARTESIAN_POINT('',(-0.146142672279203,-7.01165389862951E-5,0.266065504584291));
#14559=CARTESIAN_POINT('',(-0.146150215784492,-7.74481165901552E-5,0.258934495415711));
#14560=CARTESIAN_POINT('',(-0.14635,-1.79227059055215E-17,0.));
#14561=CARTESIAN_POINT('Ctrl Pts',(-0.146142672279203,-7.01165389862951E-5,
0.266065504584291));
#14562=CARTESIAN_POINT('Ctrl Pts',(-0.146017527260215,0.028828671850369,
0.264499287510729));
#14563=CARTESIAN_POINT('Ctrl Pts',(-0.137733916992107,0.0577936173630845,
0.262933070437168));
#14564=CARTESIAN_POINT('Ctrl Pts',(-0.121770841384076,0.0816117278206753,
0.261366853363607));
#14565=CARTESIAN_POINT('Ctrl Pts',(-0.0947991242083451,0.121855560193383,
0.258720523484505));
#14566=CARTESIAN_POINT('Ctrl Pts',(-0.0459036471244643,0.147405924851771,
0.256074193605403));
#14567=CARTESIAN_POINT('Ctrl Pts',(0.0025353607453442,0.146568017913755,
0.253427863726301));
#14568=CARTESIAN_POINT('Ctrl Pts',(0.050974368615152,0.145730110975738,
0.250781533847199));
#14569=CARTESIAN_POINT('Ctrl Pts',(0.0989569072708876,0.118503932441319,
0.248135203968097));
#14570=CARTESIAN_POINT('Ctrl Pts',(0.124520613871998,0.0773513325689396,
0.245488874088995));
#14571=CARTESIAN_POINT('Ctrl Pts',(0.150084320473109,0.0361987326965595,
0.242842544209893));
#14572=CARTESIAN_POINT('Ctrl Pts',(0.153229195019594,-0.0188802885137813,
0.240196214330791));
#14573=CARTESIAN_POINT('Ctrl Pts',(0.132515778953886,-0.0626751965094481,
0.237549884451689));
#14574=CARTESIAN_POINT('Ctrl Pts',(0.111802362888177,-0.106470104505115,
0.234903554572587));
#14575=CARTESIAN_POINT('Ctrl Pts',(0.0672306562102751,-0.138980899286108,
0.232257224693486));
#14576=CARTESIAN_POINT('Ctrl Pts',(0.0192018303028616,-0.145326878595667,
0.229610894814384));
#14577=CARTESIAN_POINT('Ctrl Pts',(-0.0288269956045516,-0.151672857905225,
0.226964564935282));
#14578=CARTESIAN_POINT('Ctrl Pts',(-0.0803129407414762,-0.131854021743351,
0.22431823505618));
#14579=CARTESIAN_POINT('Ctrl Pts',(-0.111690078002902,-0.0949417632280756,
0.221671905177078));
#14580=CARTESIAN_POINT('Ctrl Pts',(-0.133848162215005,-0.0688748557907962,
0.219803104979482));
#14581=CARTESIAN_POINT('Ctrl Pts',(-0.145978020566425,-0.0342834897603843,
0.217934304781886));
#14582=CARTESIAN_POINT('Ctrl Pts',(-0.146263250741535,0.000126870157254357,
0.21606550458429));
#14583=CARTESIAN_POINT('Ctrl Pts',(-0.146245769975643,0.000123264779366826,
0.20893449541571));
#14584=CARTESIAN_POINT('Ctrl Pts',(-0.145976242399967,-0.03366905549635,
0.210769176715493));
#14585=CARTESIAN_POINT('Ctrl Pts',(-0.134324750276972,-0.067629123606452,
0.212603858015276));
#14586=CARTESIAN_POINT('Ctrl Pts',(-0.112902327433,-0.0934976078712483,
0.214438539315059));
#14587=CARTESIAN_POINT('Ctrl Pts',(-0.0819904221256615,-0.130825044728502,
0.217085928689319));
#14588=CARTESIAN_POINT('Ctrl Pts',(-0.0307338628262512,-0.151304498698398,
0.21973331806358));
#14589=CARTESIAN_POINT('Ctrl Pts',(0.0173892134168267,-0.145555327884408,
0.22238070743784));
#14590=CARTESIAN_POINT('Ctrl Pts',(0.0655122896599044,-0.139806157070418,
0.2250280968121));
#14591=CARTESIAN_POINT('Ctrl Pts',(0.11050188284665,-0.107828361472542,
0.22767548618636));
#14592=CARTESIAN_POINT('Ctrl Pts',(0.131750448317205,-0.0642694140823833,
0.23032287556062));
#14593=CARTESIAN_POINT('Ctrl Pts',(0.15299901378776,-0.020710466692225,
0.232970264934879));
#14594=CARTESIAN_POINT('Ctrl Pts',(0.150506551542124,0.0344296324902152,
0.23561765430914));
#14595=CARTESIAN_POINT('Ctrl Pts',(0.125414737320077,0.0758938856636754,
0.2382650436834));
#14596=CARTESIAN_POINT('Ctrl Pts',(0.10032292309803,0.117358138837136,0.24091243305766));
#14597=CARTESIAN_POINT('Ctrl Pts',(0.0526317568995709,0.145146546001616,
0.24355982243192));
#14598=CARTESIAN_POINT('Ctrl Pts',(0.00418624259284972,0.146530589268381,
0.24620721180618));
#14599=CARTESIAN_POINT('Ctrl Pts',(-0.0442592717138715,0.147914632535146,
0.24885460118044));
#14600=CARTESIAN_POINT('Ctrl Pts',(-0.0934591341288551,0.122894311904195,
0.2515019905547));
#14601=CARTESIAN_POINT('Ctrl Pts',(-0.120877280418781,0.082930219442967,
0.25414937992896));
#14602=CARTESIAN_POINT('Ctrl Pts',(-0.137396572682769,0.0588520590724165,
0.255744418424543));
#14603=CARTESIAN_POINT('Ctrl Pts',(-0.146009100715185,0.0293493086505574,
0.257339456920127));
#14604=CARTESIAN_POINT('Ctrl Pts',(-0.146150215784492,-7.74481165901552E-5,
0.258934495415711));
#14605=CARTESIAN_POINT('Origin',(0.,0.,0.));
#14606=CARTESIAN_POINT('',(-0.146519404976022,-8.97763884284003E-5,0.316065504584291));
#14607=CARTESIAN_POINT('',(-0.146528765763263,-8.45393868379275E-5,0.30893449541571));
#14608=CARTESIAN_POINT('',(-0.14635,-1.79227059055215E-17,0.));
#14609=CARTESIAN_POINT('Ctrl Pts',(-0.146519404976022,-8.97763884284003E-5,
0.316065504584291));
#14610=CARTESIAN_POINT('Ctrl Pts',(-0.146208092107557,0.043076445171776,
0.313710600118674));
#14611=CARTESIAN_POINT('Ctrl Pts',(-0.125958424314353,0.0864965766126209,
0.311355695653057));
#14612=CARTESIAN_POINT('Ctrl Pts',(-0.0925183485457987,0.1137056160074,
0.309000791187441));
#14613=CARTESIAN_POINT('Ctrl Pts',(-0.0549399784004991,0.144281843189175,
0.306354461308339));
#14614=CARTESIAN_POINT('Ctrl Pts',(-0.00070450021881692,0.154386382754941,
0.303708131429237));
#14615=CARTESIAN_POINT('Ctrl Pts',(0.0453636543616171,0.139394227973128,
0.301061801550135));
#14616=CARTESIAN_POINT('Ctrl Pts',(0.0914318089420511,0.124402073191315,
0.298415471671033));
#14617=CARTESIAN_POINT('Ctrl Pts',(0.129332639921237,0.0843132240619223,
0.295769141791931));
#14618=CARTESIAN_POINT('Ctrl Pts',(0.141718340675246,0.0374769775398043,
0.293122811912829));
#14619=CARTESIAN_POINT('Ctrl Pts',(0.154104041429255,-0.00935926898231351,
0.290476482033727));
#14620=CARTESIAN_POINT('Ctrl Pts',(0.140974611958088,-0.0629429128971569,
0.287830152154626));
#14621=CARTESIAN_POINT('Ctrl Pts',(0.108339598692885,-0.0987478773661917,
0.285183822275524));
#14622=CARTESIAN_POINT('Ctrl Pts',(0.0757045854276824,-0.134552841835227,
0.282537492396422));
#14623=CARTESIAN_POINT('Ctrl Pts',(0.0235639883684441,-0.152579126858453,
0.27989116251732));
#14624=CARTESIAN_POINT('Ctrl Pts',(-0.0242166208952047,-0.144575818177467,
0.277244832638218));
#14625=CARTESIAN_POINT('Ctrl Pts',(-0.0719972301588528,-0.136572509496481,
0.274598502759116));
#14626=CARTESIAN_POINT('Ctrl Pts',(-0.115417851626912,-0.102539607111283,
0.271952172880014));
#14627=CARTESIAN_POINT('Ctrl Pts',(-0.13460418372715,-0.0580545058751705,
0.269305843000912));
#14628=CARTESIAN_POINT('Ctrl Pts',(-0.142435181350113,-0.0398976888130428,
0.268225730195372));
#14629=CARTESIAN_POINT('Ctrl Pts',(-0.146228976240411,-0.0199996345674016,
0.267145617389831));
#14630=CARTESIAN_POINT('Ctrl Pts',(-0.146142672279203,-7.01165389862951E-5,
0.266065504584291));
#14631=CARTESIAN_POINT('Ctrl Pts',(-0.146150215784492,-7.74481165901552E-5,
0.258934495415711));
#14632=CARTESIAN_POINT('Ctrl Pts',(-0.146243318595233,-0.0194921979337541,
0.259986846294387));
#14633=CARTESIAN_POINT('Ctrl Pts',(-0.142648899141753,-0.0388738684647463,
0.261039197173063));
#14634=CARTESIAN_POINT('Ctrl Pts',(-0.135204796371803,-0.0566427511368837,
0.26209154805174));
#14635=CARTESIAN_POINT('Ctrl Pts',(-0.116477735870028,-0.101343764964001,
0.264738937426));
#14636=CARTESIAN_POINT('Ctrl Pts',(-0.0733871847016099,-0.135837928326728,
0.26738632680026));
#14637=CARTESIAN_POINT('Ctrl Pts',(-0.0256708287318585,-0.144325142544676,
0.27003371617452));
#14638=CARTESIAN_POINT('Ctrl Pts',(0.0220455272378925,-0.152812356762624,
0.27268110554878));
#14639=CARTESIAN_POINT('Ctrl Pts',(0.0743876880089763,-0.135292621835792,
0.27532849492304));
#14640=CARTESIAN_POINT('Ctrl Pts',(0.10738025529095,-0.0997908762961729,
0.2779758842973));
#14641=CARTESIAN_POINT('Ctrl Pts',(0.140372822572925,-0.0642891307565533,
0.280623273671559));
#14642=CARTESIAN_POINT('Ctrl Pts',(0.154015796365789,-0.010805374604146,
0.283270663045819));
#14643=CARTESIAN_POINT('Ctrl Pts',(0.142059993874458,0.0361620845457957,
0.285918052420079));
#14644=CARTESIAN_POINT('Ctrl Pts',(0.130104191383128,0.0831295436957373,
0.288565441794339));
#14645=CARTESIAN_POINT('Ctrl Pts',(0.0925496126076039,0.123580705843213,
0.291212831168599));
#14646=CARTESIAN_POINT('Ctrl Pts',(0.0465981836912963,0.138986860871753,
0.29386022054286));
#14647=CARTESIAN_POINT('Ctrl Pts',(0.000646754774988913,0.154393015900293,
0.296507609917119));
#14648=CARTESIAN_POINT('Ctrl Pts',(-0.0537015242821025,0.144754163809898,
0.29915499929138));
#14649=CARTESIAN_POINT('Ctrl Pts',(-0.0915523499663989,0.114485393976436,
0.30180238866564));
#14650=CARTESIAN_POINT('Ctrl Pts',(-0.125542580994678,0.0873038870745135,
0.30417975758233));
#14651=CARTESIAN_POINT('Ctrl Pts',(-0.146229051243382,0.0434861464246214,
0.30655712649902));
#14652=CARTESIAN_POINT('Ctrl Pts',(-0.146528765763263,-8.45393868379275E-5,
0.30893449541571));
#14653=CARTESIAN_POINT('Origin',(0.,0.,0.));
#14654=CARTESIAN_POINT('',(-0.146416087288192,0.000126442170093593,0.366065504584291));
#14655=CARTESIAN_POINT('',(-0.146408012399712,0.000128195943346294,0.358934495415711));
#14656=CARTESIAN_POINT('',(-0.14635,-1.79227059055215E-17,0.));
#14657=CARTESIAN_POINT('Ctrl Pts',(-0.146416087288192,0.000126442170093593,
0.366065504584291));
#14658=CARTESIAN_POINT('Ctrl Pts',(-0.146499294961499,0.00925816812376314,
0.365568242605721));
#14659=CARTESIAN_POINT('Ctrl Pts',(-0.145718277739785,0.0183757049974218,
0.365070980627151));
#14660=CARTESIAN_POINT('Ctrl Pts',(-0.144021710151773,0.0273195705351122,
0.364573718648581));
#14661=CARTESIAN_POINT('Ctrl Pts',(-0.134992913071845,0.0749170536065741,
0.361927388769479));
#14662=CARTESIAN_POINT('Ctrl Pts',(-0.100034284522917,0.117595890322328,
0.359281058890377));
#14663=CARTESIAN_POINT('Ctrl Pts',(-0.0551469387876206,0.135821305661589,
0.356634729011275));
#14664=CARTESIAN_POINT('Ctrl Pts',(-0.0102595930523245,0.15404672100085,
0.353988399132173));
#14665=CARTESIAN_POINT('Ctrl Pts',(0.0445564698693406,0.147818714963618,
0.351342069253072));
#14666=CARTESIAN_POINT('Ctrl Pts',(0.0842110755700531,0.119987943896873,
0.34869573937397));
#14667=CARTESIAN_POINT('Ctrl Pts',(0.123865681270766,0.0921571728301272,
0.346049409494868));
#14668=CARTESIAN_POINT('Ctrl Pts',(0.148358829750526,0.0427236367338667,
0.343403079615766));
#14669=CARTESIAN_POINT('Ctrl Pts',(0.146479621605269,-0.00568615719458776,
0.340756749736664));
#14670=CARTESIAN_POINT('Ctrl Pts',(0.144600413460012,-0.0540959511230416,
0.338110419857562));
#14671=CARTESIAN_POINT('Ctrl Pts',(0.116348848689739,-0.101482002883689,
0.33546408997846));
#14672=CARTESIAN_POINT('Ctrl Pts',(0.0746561129649502,-0.126154971072205,
0.332817760099358));
#14673=CARTESIAN_POINT('Ctrl Pts',(0.0329633772401616,-0.150827939260721,
0.330171430220256));
#14674=CARTESIAN_POINT('Ctrl Pts',(-0.0221705294391424,-0.152787823877104,
0.327525100341154));
#14675=CARTESIAN_POINT('Ctrl Pts',(-0.0655099505772086,-0.131137554898038,
0.324878770462052));
#14676=CARTESIAN_POINT('Ctrl Pts',(-0.108849371715275,-0.109487285918972,
0.322232440582951));
#14677=CARTESIAN_POINT('Ctrl Pts',(-0.140394307312104,-0.0642268633444555,
0.319586110703849));
#14678=CARTESIAN_POINT('Ctrl Pts',(-0.14570614405606,-0.0160726946583056,
0.316939780824747));
#14679=CARTESIAN_POINT('Ctrl Pts',(-0.146291106736525,-0.0107697471190636,
0.316648355411261));
#14680=CARTESIAN_POINT('Ctrl Pts',(-0.146557930734812,-0.0054317060295066,
0.316356929997776));
#14681=CARTESIAN_POINT('Ctrl Pts',(-0.146519404976022,-8.97763884284003E-5,
0.316065504584291));
#14682=CARTESIAN_POINT('Ctrl Pts',(-0.146528765763263,-8.45393868379275E-5,
0.30893449541571));
#14683=CARTESIAN_POINT('Ctrl Pts',(-0.146562807199252,-0.00503327764821679,
0.30920451587328));
#14684=CARTESIAN_POINT('Ctrl Pts',(-0.14633385314783,-0.00997882882536714,
0.30947453633085));
#14685=CARTESIAN_POINT('Ctrl Pts',(-0.145831525524598,-0.0148964553326841,
0.309744556788419));
#14686=CARTESIAN_POINT('Ctrl Pts',(-0.140906503086998,-0.0631108472318147,
0.312391946162679));
#14687=CARTESIAN_POINT('Ctrl Pts',(-0.109703085900295,-0.108640943453547,
0.31503933553694));
#14688=CARTESIAN_POINT('Ctrl Pts',(-0.0665140418604196,-0.13063162118607,
0.3176867249112));
#14689=CARTESIAN_POINT('Ctrl Pts',(-0.0233249978205455,-0.152622298918592,
0.32033411428546));
#14690=CARTESIAN_POINT('Ctrl Pts',(0.0318496730725009,-0.151073558161906,
0.322981503659719));
#14691=CARTESIAN_POINT('Ctrl Pts',(0.0737371373950496,-0.126694801736668,
0.325628893033979));
#14692=CARTESIAN_POINT('Ctrl Pts',(0.115624601717599,-0.10231604531143,
0.328276282408239));
#14693=CARTESIAN_POINT('Ctrl Pts',(0.144224859469651,-0.0551072732176397,
0.3309236717825));
#14694=CARTESIAN_POINT('Ctrl Pts',(0.146437523492708,-0.0066925280449658,
0.33357106115676));
#14695=CARTESIAN_POINT('Ctrl Pts',(0.148650187515766,0.0417222171277085,
0.33621845053102));
#14696=CARTESIAN_POINT('Ctrl Pts',(0.124475257809829,0.0913429353792657,
0.33886583990528));
#14697=CARTESIAN_POINT('Ctrl Pts',(0.0849860939726622,0.119440788885456,
0.34151322927954));
#14698=CARTESIAN_POINT('Ctrl Pts',(0.0454969301354961,0.147538642391646,
0.344160618653799));
#14699=CARTESIAN_POINT('Ctrl Pts',(-0.00930646783289898,0.154113631152469,
0.346808008028059));
#14700=CARTESIAN_POINT('Ctrl Pts',(-0.0543213285795041,0.136154072578339,
0.349455397402319));
#14701=CARTESIAN_POINT('Ctrl Pts',(-0.0993361893261098,0.11819451400421,
0.352102786776579));
#14702=CARTESIAN_POINT('Ctrl Pts',(-0.134562512850926,0.0757004080951257,
0.35475017615084));
#14703=CARTESIAN_POINT('Ctrl Pts',(-0.143864833510727,0.0281362381501331,
0.3573975655251));
#14704=CARTESIAN_POINT('Ctrl Pts',(-0.145664973529558,0.0189318504589563,
0.357909875488637));
#14705=CARTESIAN_POINT('Ctrl Pts',(-0.146494308508217,0.00953759842677947,
0.358422185452174));
#14706=CARTESIAN_POINT('Ctrl Pts',(-0.146408012399712,0.000128195943346294,
0.358934495415711));
#14707=CARTESIAN_POINT('Origin',(0.,0.,0.));
#14708=CARTESIAN_POINT('',(-0.146110491840834,1.12683595067248E-5,0.416065504584291));
#14709=CARTESIAN_POINT('',(-0.146109756335714,8.81622270207575E-6,0.40893449541571));
#14710=CARTESIAN_POINT('',(-0.14635,-1.79227059055215E-17,0.));
#14711=CARTESIAN_POINT('Ctrl Pts',(-0.146110491840834,1.12683595067248E-5,
0.416065504584291));
#14712=CARTESIAN_POINT('Ctrl Pts',(-0.146126798292857,0.0237518011834032,
0.414779555213666));
#14713=CARTESIAN_POINT('Ctrl Pts',(-0.140669750958991,0.0474852665485293,
0.413493605843041));
#14714=CARTESIAN_POINT('Ctrl Pts',(-0.129698698951591,0.0683144158983218,
0.412207656472415));
#14715=CARTESIAN_POINT('Ctrl Pts',(-0.107121587134001,0.111178312051432,
0.409561326593314));
#14716=CARTESIAN_POINT('Ctrl Pts',(-0.0611933749717542,0.141742803557285,
0.406914996714211));
#14717=CARTESIAN_POINT('Ctrl Pts',(-0.0129361277491455,0.146018041789781,
0.40426866683511));
#14718=CARTESIAN_POINT('Ctrl Pts',(0.0353211194734639,0.150293280022276,
0.401622336956008));
#14719=CARTESIAN_POINT('Ctrl Pts',(0.0859074017564354,0.128279264981412,
0.398976007076906));
#14720=CARTESIAN_POINT('Ctrl Pts',(0.115668581836909,0.0900521576926538,
0.396329677197804));
#14721=CARTESIAN_POINT('Ctrl Pts',(0.145429761917382,0.0518250504038959,
0.393683347318702));
#14722=CARTESIAN_POINT('Ctrl Pts',(0.154365839795359,-0.0026151491327561,
0.3910370174396));
#14723=CARTESIAN_POINT('Ctrl Pts',(0.138386632036901,-0.0483503050946702,
0.388390687560498));
#14724=CARTESIAN_POINT('Ctrl Pts',(0.122407424278443,-0.094085461056585,
0.385744357681396));
#14725=CARTESIAN_POINT('Ctrl Pts',(0.0815129308835505,-0.131115573443762,
0.383098027802294));
#14726=CARTESIAN_POINT('Ctrl Pts',(0.0344212048624006,-0.142491377230642,
0.380451697923192));
#14727=CARTESIAN_POINT('Ctrl Pts',(-0.0126705211587486,-0.153867181017521,
0.37780536804409));
#14728=CARTESIAN_POINT('Ctrl Pts',(-0.0659594798061549,-0.139588676204105,
0.375159038164988));
#14729=CARTESIAN_POINT('Ctrl Pts',(-0.101054476324393,-0.106191359083811,
0.372512708285887));
#14730=CARTESIAN_POINT('Ctrl Pts',(-0.129554902927378,-0.0790696072742943,
0.370363640385355));
#14731=CARTESIAN_POINT('Ctrl Pts',(-0.146056480184715,-0.0393390709180539,
0.368214572484823));
#14732=CARTESIAN_POINT('Ctrl Pts',(-0.146416087288192,0.000126442170093593,
0.366065504584291));
#14733=CARTESIAN_POINT('Ctrl Pts',(-0.146408012399712,0.000128195943346294,
0.358934495415711));
#14734=CARTESIAN_POINT('Ctrl Pts',(-0.146048368712081,-0.0390859965171687,
0.361069574826434));
#14735=CARTESIAN_POINT('Ctrl Pts',(-0.1297855810823,-0.0785633296797545,
0.363204654237157));
#14736=CARTESIAN_POINT('Ctrl Pts',(-0.101613371150224,-0.105657280969165,
0.36533973364788));
#14737=CARTESIAN_POINT('Ctrl Pts',(-0.066681270335132,-0.139252396162569,
0.36798712302214));
#14738=CARTESIAN_POINT('Ctrl Pts',(-0.0134387509101597,-0.153808392568477,
0.370634512396399));
#14739=CARTESIAN_POINT('Ctrl Pts',(0.0337263783221333,-0.142657876135818,
0.373281901770659));
#14740=CARTESIAN_POINT('Ctrl Pts',(0.0808915075544263,-0.13150735970316,
0.375929291144919));
#14741=CARTESIAN_POINT('Ctrl Pts',(0.12197924659404,-0.0946503304319347,
0.378576680519179));
#14742=CARTESIAN_POINT('Ctrl Pts',(0.138169300408926,-0.0489692009616054,
0.38122406989344));
#14743=CARTESIAN_POINT('Ctrl Pts',(0.154359354223812,-0.00328807149127619,
0.3838714592677));
#14744=CARTESIAN_POINT('Ctrl Pts',(0.14565172281397,0.0512171581781573,
0.38651884864196));
#14745=CARTESIAN_POINT('Ctrl Pts',(0.11603494864959,0.0895802930905963,
0.38916623801622));
#14746=CARTESIAN_POINT('Ctrl Pts',(0.0864181744852101,0.127943428003035,
0.39181362739048));
#14747=CARTESIAN_POINT('Ctrl Pts',(0.0358922575662923,0.15016446815848,
0.394461016764739));
#14748=CARTESIAN_POINT('Ctrl Pts',(-0.0123993367959677,0.146065035738641,
0.397108406138999));
#14749=CARTESIAN_POINT('Ctrl Pts',(-0.0606909311582276,0.141965603318802,
0.399755795513259));
#14750=CARTESIAN_POINT('Ctrl Pts',(-0.106748202963829,0.111545698323679,
0.40240318488752));
#14751=CARTESIAN_POINT('Ctrl Pts',(-0.129474555904152,0.0687391998188283,
0.40505057426178));
#14752=CARTESIAN_POINT('Ctrl Pts',(-0.140588317483115,0.0478057390183907,
0.406345214646423));
#14753=CARTESIAN_POINT('Ctrl Pts',(-0.146122589096428,0.0239100770892618,
0.407639855031067));
#14754=CARTESIAN_POINT('Ctrl Pts',(-0.146109756335714,8.81622270207575E-6,
0.40893449541571));
#14755=CARTESIAN_POINT('Origin',(0.,0.,0.));
#14756=CARTESIAN_POINT('',(-0.146374718215768,-0.000132229735885947,0.466065504584291));
#14757=CARTESIAN_POINT('',(-0.146375609273197,-0.000132432188538665,0.458934495415711));
#14758=CARTESIAN_POINT('',(-0.14635,-1.79227059055215E-17,0.));
#14759=CARTESIAN_POINT('Ctrl Pts',(-0.146374718215768,-0.000132229735885947,
0.466065504584291));
#14760=CARTESIAN_POINT('Ctrl Pts',(-0.146022504084922,0.0379941335185874,
0.46399086782161));
#14761=CARTESIAN_POINT('Ctrl Pts',(-0.130761950520226,0.0763703265456945,
0.46191623105893));
#14762=CARTESIAN_POINT('Ctrl Pts',(-0.103994021541854,0.103314352404769,
0.45984159429625));
#14763=CARTESIAN_POINT('Ctrl Pts',(-0.0698498419286355,0.137683154682254,
0.457195264417148));
#14764=CARTESIAN_POINT('Ctrl Pts',(-0.0169824611430249,0.153451124186949,
0.454548934538046));
#14765=CARTESIAN_POINT('Ctrl Pts',(0.030409888879481,0.143401013202843,
0.451902604658944));
#14766=CARTESIAN_POINT('Ctrl Pts',(0.0778022389019875,0.133350902218736,
0.449256274779842));
#14767=CARTESIAN_POINT('Ctrl Pts',(0.119719558161389,0.0974827107458278,
0.44660994490074));
#14768=CARTESIAN_POINT('Ctrl Pts',(0.136975630157447,0.0522138743269898,
0.443963615021638));
#14769=CARTESIAN_POINT('Ctrl Pts',(0.154231702153504,0.00694503790815254,
0.441317285142536));
#14770=CARTESIAN_POINT('Ctrl Pts',(0.146826526886218,-0.0477244434566137,
0.438670955263434));
#14771=CARTESIAN_POINT('Ctrl Pts',(0.118149569579287,-0.0867714880447125,
0.436024625384332));
#14772=CARTESIAN_POINT('Ctrl Pts',(0.0894726122723542,-0.125818532632812,
0.43337829550523));
#14773=CARTESIAN_POINT('Ctrl Pts',(0.0395238729257754,-0.149243140444243,
0.430731965626129));
#14774=CARTESIAN_POINT('Ctrl Pts',(-0.00883432462988853,-0.146323499949933,
0.428085635747027));
#14775=CARTESIAN_POINT('Ctrl Pts',(-0.0571925221855517,-0.143403859455623,
0.425439305867925));
#14776=CARTESIAN_POINT('Ctrl Pts',(-0.1039601779503,-0.114139970655572,
0.422792975988823));
#14777=CARTESIAN_POINT('Ctrl Pts',(-0.127731000096207,-0.0719263758553634,
0.420146646109721));
#14778=CARTESIAN_POINT('Ctrl Pts',(-0.139950702323481,-0.0502259249733931,
0.418786265601244));
#14779=CARTESIAN_POINT('Ctrl Pts',(-0.146093241566443,-0.0251033736724598,
0.417425885092767));
#14780=CARTESIAN_POINT('Ctrl Pts',(-0.146110491840834,1.12683595067248E-5,
0.416065504584291));
#14781=CARTESIAN_POINT('Ctrl Pts',(-0.146109756335714,8.81622270207575E-6,
0.40893449541571));
#14782=CARTESIAN_POINT('Ctrl Pts',(-0.146096347589706,-0.0249652282079418,
0.410287244405327));
#14783=CARTESIAN_POINT('Ctrl Pts',(-0.140026707259891,-0.049945385460595,
0.411639993394943));
#14784=CARTESIAN_POINT('Ctrl Pts',(-0.127937780377622,-0.0715588049813403,
0.412992742384559));
#14785=CARTESIAN_POINT('Ctrl Pts',(-0.104279217835726,-0.113857219262079,
0.415640131758819));
#14786=CARTESIAN_POINT('Ctrl Pts',(-0.0575666586768896,-0.14326095580898,
0.41828752113308));
#14787=CARTESIAN_POINT('Ctrl Pts',(-0.00919685447762893,-0.146301592903247,
0.42093491050734));
#14788=CARTESIAN_POINT('Ctrl Pts',(0.039172949721632,-0.149342229997515,
0.4235822998816));
#14789=CARTESIAN_POINT('Ctrl Pts',(0.089199998961318,-0.126019767639148,
0.426229689255859));
#14790=CARTESIAN_POINT('Ctrl Pts',(0.117969334952632,-0.0870170915920772,
0.428877078630119));
#14791=CARTESIAN_POINT('Ctrl Pts',(0.146738670943946,-0.0480144155450057,
0.431524468004379));
#14792=CARTESIAN_POINT('Ctrl Pts',(0.154250293686888,0.00666847419077017,
0.43417185737864));
#14793=CARTESIAN_POINT('Ctrl Pts',(0.137063494116028,0.051984005222912,
0.4368192467529));
#14794=CARTESIAN_POINT('Ctrl Pts',(0.119876694545168,0.0972995362550541,
0.43946663612716));
#14795=CARTESIAN_POINT('Ctrl Pts',(0.0779914726605056,0.133247708583562,
0.442114025501419));
#14796=CARTESIAN_POINT('Ctrl Pts',(0.0305934116013849,0.143362412733947,
0.444761414875679));
#14797=CARTESIAN_POINT('Ctrl Pts',(-0.0168046494577345,0.153477116884331,
0.447408804249939));
#14798=CARTESIAN_POINT('Ctrl Pts',(-0.0697155496913122,0.137758352856595,
0.4500561936242));
#14799=CARTESIAN_POINT('Ctrl Pts',(-0.103903378920715,0.103406122000434,
0.45270358299846));
#14800=CARTESIAN_POINT('Ctrl Pts',(-0.130724942802416,0.0764555792150183,
0.45478055380421));
#14801=CARTESIAN_POINT('Ctrl Pts',(-0.146022533856355,0.0380362146017157,
0.45685752460996));
#14802=CARTESIAN_POINT('Ctrl Pts',(-0.146375609273197,-0.000132432188538665,
0.458934495415711));
#14803=CARTESIAN_POINT('Origin',(0.,0.,0.));
#14804=CARTESIAN_POINT('',(-0.146548608312775,6.99729089778146E-5,0.516065504584291));
#14805=CARTESIAN_POINT('',(-0.146550766805835,6.86360251013434E-5,0.508934495415711));
#14806=CARTESIAN_POINT('',(-0.14635,-1.79227059055215E-17,0.));
#14807=CARTESIAN_POINT('Ctrl Pts',(-0.146548608312775,6.99729089778146E-5,
0.516065504584291));
#14808=CARTESIAN_POINT('Ctrl Pts',(-0.146572081366671,0.00404546554386884,
0.515848510308657));
#14809=CARTESIAN_POINT('Ctrl Pts',(-0.146424333269732,0.00801918670503405,
0.515631516033023));
#14810=CARTESIAN_POINT('Ctrl Pts',(-0.146099725131082,0.0119784074854107,
0.51541452175739));
#14811=CARTESIAN_POINT('Ctrl Pts',(-0.142141002193345,0.06026265009261,
0.512768191878288));
#14812=CARTESIAN_POINT('Ctrl Pts',(-0.111878319621163,0.106390286678145,
0.510121861999186));
#14813=CARTESIAN_POINT('Ctrl Pts',(-0.069163383343408,0.129247972261684,
0.507475532120084));
#14814=CARTESIAN_POINT('Ctrl Pts',(-0.0264484470656534,0.152105657845224,
0.504829202240982));
#14815=CARTESIAN_POINT('Ctrl Pts',(0.0287187429176733,0.151693392426768,
0.50218287236188));
#14816=CARTESIAN_POINT('Ctrl Pts',(0.07108729581893,0.128199876374419,0.499536542482778));
#14817=CARTESIAN_POINT('Ctrl Pts',(0.113455848720186,0.10470636032207,0.496890212603677));
#14818=CARTESIAN_POINT('Ctrl Pts',(0.143025764539373,0.0581315936358261,
0.494243882724575));
#14819=CARTESIAN_POINT('Ctrl Pts',(0.146262427589597,0.00979357977770552,
0.491597552845473));
#14820=CARTESIAN_POINT('Ctrl Pts',(0.149499090639821,-0.0385444340804161,
0.488951222966371));
#14821=CARTESIAN_POINT('Ctrl Pts',(0.126402500921083,-0.0886456951104151,
0.486304893087269));
#14822=CARTESIAN_POINT('Ctrl Pts',(0.087544330920799,-0.117578067907642,
0.483658563208167));
#14823=CARTESIAN_POINT('Ctrl Pts',(0.0486861609205161,-0.146510440704867,
0.481012233329065));
#14824=CARTESIAN_POINT('Ctrl Pts',(-0.00593358936131212,-0.154273925269321,
0.478365903449963));
#14825=CARTESIAN_POINT('Ctrl Pts',(-0.0513146009011563,-0.137315052574797,
0.475719573570861));
#14826=CARTESIAN_POINT('Ctrl Pts',(-0.0966956124410008,-0.120356179880273,
0.473073243691759));
#14827=CARTESIAN_POINT('Ctrl Pts',(-0.132837885238862,-0.078674949926771,
0.470426913812657));
#14828=CARTESIAN_POINT('Ctrl Pts',(-0.14319853241738,-0.0313495174248821,
0.467780583933555));
#14829=CARTESIAN_POINT('Ctrl Pts',(-0.145436768368387,-0.0211256884885646,
0.467208890817134));
#14830=CARTESIAN_POINT('Ctrl Pts',(-0.146471775395962,-0.0106384445195334,
0.466637197700712));
#14831=CARTESIAN_POINT('Ctrl Pts',(-0.146374718215768,-0.000132229735885947,
0.466065504584291));
#14832=CARTESIAN_POINT('Ctrl Pts',(-0.146375609273197,-0.000132432188538665,
0.458934495415711));
#14833=CARTESIAN_POINT('Ctrl Pts',(-0.146472577787773,-0.0106150565970108,
0.45950491398422));
#14834=CARTESIAN_POINT('Ctrl Pts',(-0.145442327125792,-0.021078770125739,
0.46007533255273));
#14835=CARTESIAN_POINT('Ctrl Pts',(-0.143213999951756,-0.0312807998000163,
0.460645751121239));
#14836=CARTESIAN_POINT('Ctrl Pts',(-0.132872033528166,-0.0786297930597184,
0.463293140495499));
#14837=CARTESIAN_POINT('Ctrl Pts',(-0.0967233424557573,-0.120342081894533,
0.465940529869759));
#14838=CARTESIAN_POINT('Ctrl Pts',(-0.0513258840937604,-0.13731129538499,
0.46858791924402));
#14839=CARTESIAN_POINT('Ctrl Pts',(-0.00592842573176499,-0.154280508875447,
0.47123530861828));
#14840=CARTESIAN_POINT('Ctrl Pts',(0.0487177999198187,-0.146506647021548,
0.47388269799254));
#14841=CARTESIAN_POINT('Ctrl Pts',(0.0875820145025328,-0.117550537871965,
0.476530087366799));
#14842=CARTESIAN_POINT('Ctrl Pts',(0.126446229085248,-0.0885944287223814,
0.47917747674106));
#14843=CARTESIAN_POINT('Ctrl Pts',(0.149528432599094,-0.0384560722771122,
0.481824866115319));
#14844=CARTESIAN_POINT('Ctrl Pts',(0.146255790172295,0.0098985887573764,
0.484472255489579));
#14845=CARTESIAN_POINT('Ctrl Pts',(0.142983147745498,0.0582532497918637,
0.487119644863839));
#14846=CARTESIAN_POINT('Ctrl Pts',(0.113355659378058,0.10482421541557,0.4897670342381));
#14847=CARTESIAN_POINT('Ctrl Pts',(0.0709442366160257,0.128279591164298,
0.49241442361236));
#14848=CARTESIAN_POINT('Ctrl Pts',(0.0285328138539934,0.151734966913027,
0.49506181298662));
#14849=CARTESIAN_POINT('Ctrl Pts',(-0.0266625433026316,0.152074752786777,
0.497709202360879));
#14850=CARTESIAN_POINT('Ctrl Pts',(-0.0693595260588707,0.129143309401606,
0.500356591735139));
#14851=CARTESIAN_POINT('Ctrl Pts',(-0.11205650881511,0.106211866016435,
0.503003981109399));
#14852=CARTESIAN_POINT('Ctrl Pts',(-0.142255117170964,0.060009193372344,
0.505651370483659));
#14853=CARTESIAN_POINT('Ctrl Pts',(-0.146122837288996,0.0116984888307781,
0.50829875985792));
#14854=CARTESIAN_POINT('Ctrl Pts',(-0.146432431239741,0.00783142983325791,
0.508510671710517));
#14855=CARTESIAN_POINT('Ctrl Pts',(-0.14657331536999,0.00395086404934249,
0.508722583563114));
#14856=CARTESIAN_POINT('Ctrl Pts',(-0.146550766805835,6.86360251013434E-5,
0.508934495415711));
#14857=CARTESIAN_POINT('Origin',(0.,0.,0.));
#14858=CARTESIAN_POINT('',(-0.146165204287215,8.83645032875094E-5,0.566065504584291));
#14859=CARTESIAN_POINT('',(-0.146168951232552,9.12430751481418E-5,0.558934495415711));
#14860=CARTESIAN_POINT('',(-0.14635,-1.79227059055215E-17,0.));
#14861=CARTESIAN_POINT('Ctrl Pts',(-0.146165204287215,8.83645032875094E-5,
0.566065504584291));
#14862=CARTESIAN_POINT('Ctrl Pts',(-0.146267412293664,0.0186373661349918,
0.565059822916602));
#14863=CARTESIAN_POINT('Ctrl Pts',(-0.142994166834961,0.0371516370495788,
0.564054141248913));
#14864=CARTESIAN_POINT('Ctrl Pts',(-0.136179985035193,0.0542551712289143,
0.563048459581224));
#14865=CARTESIAN_POINT('Ctrl Pts',(-0.118249288396568,0.0992610562830057,
0.560402129702122));
#14866=CARTESIAN_POINT('Ctrl Pts',(-0.0758005933416487,0.134498778989873,
0.55775579982302));
#14867=CARTESIAN_POINT('Ctrl Pts',(-0.0282633354322908,0.143839479279877,
0.555109469943918));
#14868=CARTESIAN_POINT('Ctrl Pts',(0.0192739224770691,0.153180179569881,
0.552463140064816));
#14869=CARTESIAN_POINT('Ctrl Pts',(0.0718997432408687,0.136623857443018,
0.549816810185715));
#14870=CARTESIAN_POINT('Ctrl Pts',(0.105526460745998,0.101748602013432,
0.547170480306613));
#14871=CARTESIAN_POINT('Ctrl Pts',(0.139153178251127,0.0668733465838454,
0.544524150427511));
#14872=CARTESIAN_POINT('Ctrl Pts',(0.153780792497586,0.0136791578515372,
0.541877820548409));
#14873=CARTESIAN_POINT('Ctrl Pts',(0.142714014311998,-0.0334861471092027,
0.539231490669307));
#14874=CARTESIAN_POINT('Ctrl Pts',(0.13164723612641,-0.0806514520699426,
0.536585160790205));
#14875=CARTESIAN_POINT('Ctrl Pts',(0.0948860655087725,-0.121787873259113,
0.533938830911103));
#14876=CARTESIAN_POINT('Ctrl Pts',(0.0492566686055307,-0.138066623508903,
0.531292501032001));
#14877=CARTESIAN_POINT('Ctrl Pts',(0.00362727170228945,-0.154345373758693,
0.528646171152899));
#14878=CARTESIAN_POINT('Ctrl Pts',(-0.050870351486557,-0.145766453069103,
0.525999841273797));
#14879=CARTESIAN_POINT('Ctrl Pts',(-0.089291781429334,-0.116256568409877,
0.523353511394695));
#14880=CARTESIAN_POINT('Ctrl Pts',(-0.124562723435938,-0.0891664410515947,
0.520924175791227));
#14881=CARTESIAN_POINT('Ctrl Pts',(-0.146285818313441,-0.0444372186796531,
0.518494840187759));
#14882=CARTESIAN_POINT('Ctrl Pts',(-0.146548608312775,6.99729089778146E-5,
0.516065504584291));
#14883=CARTESIAN_POINT('Ctrl Pts',(-0.146550766805835,6.86360251013434E-5,
0.508934495415711));
#14884=CARTESIAN_POINT('Ctrl Pts',(-0.146291618860727,-0.0445493453248537,
0.511369972937373));
#14885=CARTESIAN_POINT('Ctrl Pts',(-0.124445252016267,-0.0893868858389474,
0.513805450459036));
#14886=CARTESIAN_POINT('Ctrl Pts',(-0.0890226177929609,-0.116463349340462,
0.516240927980699));
#14887=CARTESIAN_POINT('Ctrl Pts',(-0.0505178462986829,-0.145895746531099,
0.518888317354959));
#14888=CARTESIAN_POINT('Ctrl Pts',(0.00402852857008221,-0.154341804473332,
0.52153570672922));
#14889=CARTESIAN_POINT('Ctrl Pts',(0.0496314652424392,-0.137932794781367,
0.52418309610348));
#14890=CARTESIAN_POINT('Ctrl Pts',(0.0952344019147948,-0.121523785089403,
0.52683048547774));
#14891=CARTESIAN_POINT('Ctrl Pts',(0.131893900390741,-0.0802597077632436,
0.529477874851999));
#14892=CARTESIAN_POINT('Ctrl Pts',(0.14281802728161,-0.0330416298281342,
0.532125264226259));
#14893=CARTESIAN_POINT('Ctrl Pts',(0.153742154172479,0.0141764481069759,
0.53477265360052));
#14894=CARTESIAN_POINT('Ctrl Pts',(0.138930909478268,0.0673485266510362,
0.53742004297478));
#14895=CARTESIAN_POINT('Ctrl Pts',(0.105168604077417,0.102119062543277,
0.54006743234904));
#14896=CARTESIAN_POINT('Ctrl Pts',(0.0714062986765666,0.136889598435517,
0.5427148217233));
#14897=CARTESIAN_POINT('Ctrl Pts',(0.018692932569077,0.153258591675938,
0.545362211097559));
#14898=CARTESIAN_POINT('Ctrl Pts',(-0.0288260648428939,0.143728202535144,
0.548009600471819));
#14899=CARTESIAN_POINT('Ctrl Pts',(-0.0763450622548654,0.13419781339435,
0.550656989846079));
#14900=CARTESIAN_POINT('Ctrl Pts',(-0.118669690971318,0.0987680418723385,
0.55330437922034));
#14901=CARTESIAN_POINT('Ctrl Pts',(-0.136413096952957,0.0536675432455532,
0.5559517685946));
#14902=CARTESIAN_POINT('Ctrl Pts',(-0.143076734904351,0.036729792140314,
0.556946010868304));
#14903=CARTESIAN_POINT('Ctrl Pts',(-0.146273385252938,0.0184280612467595,
0.557940253142007));
#14904=CARTESIAN_POINT('Ctrl Pts',(-0.146168951232552,9.12430751481418E-5,
0.558934495415711));
#14905=CARTESIAN_POINT('Origin',(0.,0.,0.));
#14906=CARTESIAN_POINT('',(-0.146227179098081,-0.000117664897458569,0.616065504584291));
#14907=CARTESIAN_POINT('',(-0.146218520919543,-0.000115076211918358,0.608934495415711));
#14908=CARTESIAN_POINT('',(-0.14635,-1.79227059055215E-17,0.));
#14909=CARTESIAN_POINT('Ctrl Pts',(-0.146227179098081,-0.000117664897458569,
0.616065504584291));
#14910=CARTESIAN_POINT('Ctrl Pts',(-0.145977603365176,0.0329427899635141,
0.614271135524546));
#14911=CARTESIAN_POINT('Ctrl Pts',(-0.134874795495675,0.0661550248562671,
0.612476766464802));
#14912=CARTESIAN_POINT('Ctrl Pts',(-0.114309815624116,0.091770790457776,
0.610682397405058));
#14913=CARTESIAN_POINT('Ctrl Pts',(-0.0839806476072558,0.129548841477563,
0.608036067525956));
#14914=CARTESIAN_POINT('Ctrl Pts',(-0.0330710111925292,0.150804375664025,
0.605389737646855));
#14915=CARTESIAN_POINT('Ctrl Pts',(0.0151169520838501,0.145808400611758,
0.602743407767753));
#14916=CARTESIAN_POINT('Ctrl Pts',(0.0633049153602295,0.140812425559491,
0.600097077888651));
#14917=CARTESIAN_POINT('Ctrl Pts',(0.108771205498262,0.109564941268491,
0.597450748009549));
#14918=CARTESIAN_POINT('Ctrl Pts',(0.130705186191441,0.0663684129079872,
0.594804418130447));
#14919=CARTESIAN_POINT('Ctrl Pts',(0.152639166884621,0.023171884547483,
0.592158088251345));
#14920=CARTESIAN_POINT('Ctrl Pts',(0.151040838132949,-0.0319736878825246,
0.589511758372243));
#14921=CARTESIAN_POINT('Ctrl Pts',(0.126641780152193,-0.0738273082886534,
0.586865428493141));
#14922=CARTESIAN_POINT('Ctrl Pts',(0.102242722171437,-0.115680928694782,
0.584219098614039));
#14923=CARTESIAN_POINT('Ctrl Pts',(0.0550429349615966,-0.14424259707703,
0.581572768734937));
#14924=CARTESIAN_POINT('Ctrl Pts',(0.00664650371163741,-0.14643918846291,
0.578926438855836));
#14925=CARTESIAN_POINT('Ctrl Pts',(-0.0417499275383225,-0.148635779848789,
0.576280108976733));
#14926=CARTESIAN_POINT('Ctrl Pts',(-0.0913430028284016,-0.1244672942383,
0.573633779097631));
#14927=CARTESIAN_POINT('Ctrl Pts',(-0.119433191362276,-0.0849960277323969,
0.570987449218529));
#14928=CARTESIAN_POINT('Ctrl Pts',(-0.136848298201485,-0.0605249807527623,
0.569346801007117));
#14929=CARTESIAN_POINT('Ctrl Pts',(-0.145998464265635,-0.0301720919893573,
0.567706152795704));
#14930=CARTESIAN_POINT('Ctrl Pts',(-0.146165204287215,8.83645032875094E-5,
0.566065504584291));
#14931=CARTESIAN_POINT('Ctrl Pts',(-0.146168951232552,9.12430751481418E-5,
0.558934495415711));
#14932=CARTESIAN_POINT('Ctrl Pts',(-0.145995306636495,-0.0303977620653178,
0.560587642516267));
#14933=CARTESIAN_POINT('Ctrl Pts',(-0.136695352934655,-0.0609837708898569,
0.562240789616823));
#14934=CARTESIAN_POINT('Ctrl Pts',(-0.119031718004195,-0.0855580991331628,
0.563893936717379));
#14935=CARTESIAN_POINT('Ctrl Pts',(-0.090744749826965,-0.124912017153538,
0.566541326091639));
#14936=CARTESIAN_POINT('Ctrl Pts',(-0.0410086302256792,-0.148848627462727,
0.5691887154659));
#14937=CARTESIAN_POINT('Ctrl Pts',(0.00739494322942312,-0.146403732988417,
0.57183610484016));
#14938=CARTESIAN_POINT('Ctrl Pts',(0.0557985166845234,-0.143958838514108,
0.57448349421442));
#14939=CARTESIAN_POINT('Ctrl Pts',(0.10286954399344,-0.1151324392563,0.57713088358868));
#14940=CARTESIAN_POINT('Ctrl Pts',(0.127047076753504,-0.0731285067993286,
0.579778272962939));
#14941=CARTESIAN_POINT('Ctrl Pts',(0.151224609513568,-0.031124574342357,
0.5824256623372));
#14942=CARTESIAN_POINT('Ctrl Pts',(0.15250864772478,0.0240568913137802,
0.58507305171146));
#14943=CARTESIAN_POINT('Ctrl Pts',(0.130311035929276,0.0671399443948921,
0.58772044108572));
#14944=CARTESIAN_POINT('Ctrl Pts',(0.108113424133771,0.110222997476006,
0.59036783045998));
#14945=CARTESIAN_POINT('Ctrl Pts',(0.0624341623315493,0.141207637982093,
0.593015219834239));
#14946=CARTESIAN_POINT('Ctrl Pts',(0.0141966988324609,0.145901308974836,
0.595662609208499));
#14947=CARTESIAN_POINT('Ctrl Pts',(-0.0340407646666261,0.150594979967579,
0.598309998582759));
#14948=CARTESIAN_POINT('Ctrl Pts',(-0.0848364298625779,0.128997681446978,
0.60095738795702));
#14949=CARTESIAN_POINT('Ctrl Pts',(-0.114923272877171,0.091002085522857,
0.60360477733128));
#14950=CARTESIAN_POINT('Ctrl Pts',(-0.135113526827902,0.0655045372973676,
0.60538135002609));
#14951=CARTESIAN_POINT('Ctrl Pts',(-0.14597798884013,0.0326223532682757,
0.6071579227209));
#14952=CARTESIAN_POINT('Ctrl Pts',(-0.146218520919543,-0.000115076211918358,
0.608934495415711));
#14953=CARTESIAN_POINT('Origin',(0.,0.,0.));
#14954=CARTESIAN_POINT('',(-0.146586033401767,-2.15382961294558E-5,0.66606550458429));
#14955=CARTESIAN_POINT('',(-0.146582846697157,-3.00215943766004E-5,0.65893449541571));
#14956=CARTESIAN_POINT('',(-0.14635,-1.79227059055215E-17,0.));
#14957=CARTESIAN_POINT('Ctrl Pts',(-0.146586033401767,-2.15382961294558E-5,
0.66606550458429));
#14958=CARTESIAN_POINT('Ctrl Pts',(-0.146488810225965,0.0472697707580183,
0.663482448132491));
#14959=CARTESIAN_POINT('Ctrl Pts',(-0.121516563758978,0.0946492637554097,
0.660899391680692));
#14960=CARTESIAN_POINT('Ctrl Pts',(-0.0824084263440199,0.121233094478226,
0.658316335228893));
#14961=CARTESIAN_POINT('Ctrl Pts',(-0.0423423130056393,0.148468111155377,
0.655670005349791));
#14962=CARTESIAN_POINT('Ctrl Pts',(0.0125607065496858,0.153876184485078,
0.653023675470689));
#14963=CARTESIAN_POINT('Ctrl Pts',(0.0571706564953393,0.134981954220393,
0.650377345591587));
#14964=CARTESIAN_POINT('Ctrl Pts',(0.101780606440992,0.116087723955709,
0.647731015712485));
#14965=CARTESIAN_POINT('Ctrl Pts',(0.136097486776972,0.0728911900966409,
0.645084685833384));
#14966=CARTESIAN_POINT('Ctrl Pts',(0.144413921474191,0.0251640857912735,
0.642438355954282));
#14967=CARTESIAN_POINT('Ctrl Pts',(0.152730356171409,-0.0225630185140953,
0.63979202607518));
#14968=CARTESIAN_POINT('Ctrl Pts',(0.135046345229863,-0.0748206932657649,
0.637145696196077));
#14969=CARTESIAN_POINT('Ctrl Pts',(0.0994561386758346,-0.10768977857233,
0.634499366316975));
#14970=CARTESIAN_POINT('Ctrl Pts',(0.0638659321218069,-0.140558863878895,
0.631853036437873));
#14971=CARTESIAN_POINT('Ctrl Pts',(0.0103695299552984,-0.154039359740357,
0.629206706558772));
#14972=CARTESIAN_POINT('Ctrl Pts',(-0.0365469229059137,-0.141961031115491,
0.62656037667967));
#14973=CARTESIAN_POINT('Ctrl Pts',(-0.0834633757671259,-0.129882702490626,
0.623914046800568));
#14974=CARTESIAN_POINT('Ctrl Pts',(-0.123799879323041,-0.0922455493794331,
0.621267716921466));
#14975=CARTESIAN_POINT('Ctrl Pts',(-0.139093781291504,-0.0462766888972804,
0.618621387042364));
#14976=CARTESIAN_POINT('Ctrl Pts',(-0.14401750805555,-0.0314774500153124,
0.617769426223006));
#14977=CARTESIAN_POINT('Ctrl Pts',(-0.14634567687575,-0.0158146654998378,
0.616917465403648));
#14978=CARTESIAN_POINT('Ctrl Pts',(-0.146227179098081,-0.000117664897458569,
0.616065504584291));
#14979=CARTESIAN_POINT('Ctrl Pts',(-0.146218520919543,-0.000115076211918358,
0.608934495415711));
#14980=CARTESIAN_POINT('Ctrl Pts',(-0.1463364217222,-0.0161618722236638,
0.60980531209516));
#14981=CARTESIAN_POINT('Ctrl Pts',(-0.143901781624712,-0.032173889023867,
0.61067612877461));
#14982=CARTESIAN_POINT('Ctrl Pts',(-0.138761720114909,-0.0472643972675185,
0.611546945454059));
#14983=CARTESIAN_POINT('Ctrl Pts',(-0.123135303504819,-0.0931413908061287,
0.614194334828319));
#14984=CARTESIAN_POINT('Ctrl Pts',(-0.0825044494514074,-0.130501484555709,
0.616841724202579));
#14985=CARTESIAN_POINT('Ctrl Pts',(-0.0354801761942514,-0.142231836504824,
0.619489113576839));
#14986=CARTESIAN_POINT('Ctrl Pts',(0.0115440970629072,-0.15396218845394,
0.6221365029511));
#14987=CARTESIAN_POINT('Ctrl Pts',(0.0649617895238099,-0.140062798602586,
0.624783892325359));
#14988=CARTESIAN_POINT('Ctrl Pts',(0.100304854137336,-0.106900301471969,
0.627431281699619));
#14989=CARTESIAN_POINT('Ctrl Pts',(0.135647918750861,-0.0737378043413545,
0.630078671073879));
#14990=CARTESIAN_POINT('Ctrl Pts',(0.15291635551701,-0.0213121999314781,
0.63272606044814));
#14991=CARTESIAN_POINT('Ctrl Pts',(0.144200333369931,0.026362891994447,
0.6353734498224));
#14992=CARTESIAN_POINT('Ctrl Pts',(0.135484311222852,0.0740379839203748,
0.63802083919666));
#14993=CARTESIAN_POINT('Ctrl Pts',(0.100783830162543,0.11696256336235,0.640668228570919));
#14994=CARTESIAN_POINT('Ctrl Pts',(0.055993492972559,0.135474968031154,
0.643315617945179));
#14995=CARTESIAN_POINT('Ctrl Pts',(0.0112031557825773,0.153987372699956,
0.64596300731944));
#14996=CARTESIAN_POINT('Ctrl Pts',(-0.04367703753708,0.148087602595587,
0.6486103966937));
#14997=CARTESIAN_POINT('Ctrl Pts',(-0.0835091394177698,0.120478055479053,
0.65125778606796));
#14998=CARTESIAN_POINT('Ctrl Pts',(-0.122009894390588,0.0937913289882395,
0.653816689183877));
#14999=CARTESIAN_POINT('Ctrl Pts',(-0.146451680634158,0.0468218259492564,
0.656375592299793));
#15000=CARTESIAN_POINT('Ctrl Pts',(-0.146582846697157,-3.00215943766004E-5,
0.65893449541571));
#15001=CARTESIAN_POINT('Origin',(0.,0.,0.));
#15002=CARTESIAN_POINT('',(-0.146290249280603,0.000131112932912382,0.716065504584291));
#15003=CARTESIAN_POINT('',(-0.146307221518699,0.000133045872591754,0.708934495415711));
#15004=CARTESIAN_POINT('',(-0.14635,-1.79227059055215E-17,0.));
#15005=CARTESIAN_POINT('Ctrl Pts',(-0.146290249280603,0.000131112932912382,
0.716065504584291));
#15006=CARTESIAN_POINT('Ctrl Pts',(-0.146406294125046,0.0134819654399978,
0.715340090619538));
#15007=CARTESIAN_POINT('Ctrl Pts',(-0.144729088574721,0.0268041890186768,
0.714614676654786));
#15008=CARTESIAN_POINT('Ctrl Pts',(-0.141142411757643,0.0395908011096033,
0.713889262690033));
#15009=CARTESIAN_POINT('Ctrl Pts',(-0.128058117149462,0.0862367098911347,
0.711242932810931));
#15010=CARTESIAN_POINT('Ctrl Pts',(-0.0895623832093418,0.125754646095387,
0.708596602931829));
#15011=CARTESIAN_POINT('Ctrl Pts',(-0.0432753130058998,0.140056628595385,
0.705950273052727));
#15012=CARTESIAN_POINT('Ctrl Pts',(0.00301175719754219,0.154358611095384,
0.703303943173625));
#15013=CARTESIAN_POINT('Ctrl Pts',(0.0570901636643063,0.143444639891129,
0.700657613294523));
#15014=CARTESIAN_POINT('Ctrl Pts',(0.0942073689518517,0.11231021130972,
0.698011283415421));
#15015=CARTESIAN_POINT('Ctrl Pts',(0.131324574239397,0.0811757827283121,
0.695364953536319));
#15016=CARTESIAN_POINT('Ctrl Pts',(0.151480578347723,0.0298208967697505,
0.692718623657217));
#15017=CARTESIAN_POINT('Ctrl Pts',(0.145449661086834,-0.0182485073085286,
0.690072293778115));
#15018=CARTESIAN_POINT('Ctrl Pts',(0.139418743825945,-0.0663179113868083,
0.687425963899014));
#15019=CARTESIAN_POINT('Ctrl Pts',(0.107200905195838,-0.111101833584806,
0.684779634019911));
#15020=CARTESIAN_POINT('Ctrl Pts',(0.0635427568131047,-0.132101968137704,
0.68213330414081));
#15021=CARTESIAN_POINT('Ctrl Pts',(0.0198846084303716,-0.153102102690602,
0.679486974261708));
#15022=CARTESIAN_POINT('Ctrl Pts',(-0.0352138497049885,-0.150318449598402,
0.676840644382606));
#15023=CARTESIAN_POINT('Ctrl Pts',(-0.0765331864534889,-0.125025130675956,
0.674194314503504));
#15024=CARTESIAN_POINT('Ctrl Pts',(-0.117852523201989,-0.0997318117535095,
0.671547984624402));
#15025=CARTESIAN_POINT('Ctrl Pts',(-0.14539273856363,-0.0519288270008166,
0.6689016547453));
#15026=CARTESIAN_POINT('Ctrl Pts',(-0.146548242683733,-0.00349635461217019,
0.666255324866198));
#15027=CARTESIAN_POINT('Ctrl Pts',(-0.146575870647472,-0.00233834005587287,
0.666192051438896));
#15028=CARTESIAN_POINT('Ctrl Pts',(-0.146588414938392,-0.00117996563262623,
0.666128778011593));
#15029=CARTESIAN_POINT('Ctrl Pts',(-0.146586033401767,-2.15382961294558E-5,
0.66606550458429));
#15030=CARTESIAN_POINT('Ctrl Pts',(-0.146582846697157,-3.00215943766004E-5,
0.65893449541571));
#15031=CARTESIAN_POINT('Ctrl Pts',(-0.146587382388275,-0.00165014728799839,
0.659022981674053));
#15032=CARTESIAN_POINT('Ctrl Pts',(-0.146562848415234,-0.00327013229389975,
0.659111467932396));
#15033=CARTESIAN_POINT('Ctrl Pts',(-0.146508820881567,-0.00488913307276392,
0.659199954190739));
#15034=CARTESIAN_POINT('Ctrl Pts',(-0.144892390022949,-0.0533274503793473,
0.661847343564999));
#15035=CARTESIAN_POINT('Ctrl Pts',(-0.116875517863988,-0.100884760863813,
0.66449473293926));
#15036=CARTESIAN_POINT('Ctrl Pts',(-0.0752913709948059,-0.125777373450206,
0.66714212231352));
#15037=CARTESIAN_POINT('Ctrl Pts',(-0.0337072241256252,-0.150669986036599,
0.66978951168778));
#15038=CARTESIAN_POINT('Ctrl Pts',(0.021444197453776,-0.15289790072492,
0.672436901062039));
#15039=CARTESIAN_POINT('Ctrl Pts',(0.0649007096996251,-0.131440618146733,
0.675084290436299));
#15040=CARTESIAN_POINT('Ctrl Pts',(0.108357221945475,-0.109983335568545,
0.677731679810559));
#15041=CARTESIAN_POINT('Ctrl Pts',(0.140118824857774,-0.0648408557238465,
0.68037906918482));
#15042=CARTESIAN_POINT('Ctrl Pts',(0.145637072805965,-0.0166907532130915,
0.68302645855908));
#15043=CARTESIAN_POINT('Ctrl Pts',(0.151155320754156,0.031459349297663,
0.68567384793334));
#15044=CARTESIAN_POINT('Ctrl Pts',(0.130430213738242,0.0826170744744734,
0.688321237307599));
#15045=CARTESIAN_POINT('Ctrl Pts',(0.0929549153570804,0.113349556369966,
0.690968626681859));
#15046=CARTESIAN_POINT('Ctrl Pts',(0.0554796169759186,0.14408203826546,
0.693616016056119));
#15047=CARTESIAN_POINT('Ctrl Pts',(0.00125412722950909,0.154389276879634,
0.69626340543038));
#15048=CARTESIAN_POINT('Ctrl Pts',(-0.0448834941801804,0.139550027475769,
0.69891079480464));
#15049=CARTESIAN_POINT('Ctrl Pts',(-0.0910211155898686,0.124710778071904,
0.7015581841789));
#15050=CARTESIAN_POINT('Ctrl Pts',(-0.129070868662838,0.0847250406500019,
0.704205573553159));
#15051=CARTESIAN_POINT('Ctrl Pts',(-0.141604011991841,0.0379083368947344,
0.706852962927419));
#15052=CARTESIAN_POINT('Ctrl Pts',(-0.144888775625201,0.0256383259412015,
0.707546807090183));
#15053=CARTESIAN_POINT('Ctrl Pts',(-0.146420824649375,0.0128991016161637,
0.708240651252947));
#15054=CARTESIAN_POINT('Ctrl Pts',(-0.146307221518699,0.000133045872591754,
0.708934495415711));
#15055=CARTESIAN_POINT('Origin',(0.,0.,0.));
#15056=CARTESIAN_POINT('',(-0.1461301977291,-5.61458017395017E-5,0.766065504584291));
#15057=CARTESIAN_POINT('',(-0.14612241379348,-4.54149644099216E-5,0.758934495415711));
#15058=CARTESIAN_POINT('',(-0.14635,-1.79227059055215E-17,0.));
#15059=CARTESIAN_POINT('Ctrl Pts',(-0.1461301977291,-5.61458017395017E-5,
0.766065504584291));
#15060=CARTESIAN_POINT('Ctrl Pts',(-0.14603380141711,0.0278870014676159,
0.764551403227483));
#15061=CARTESIAN_POINT('Ctrl Pts',(-0.138327245009168,0.0558793842949389,
0.763037301870675));
#15062=CARTESIAN_POINT('Ctrl Pts',(-0.123350675409043,0.079203679241543,
0.761523200513867));
#15063=CARTESIAN_POINT('Ctrl Pts',(-0.0971747899961838,0.119969628197767,
0.758876870634766));
#15064=CARTESIAN_POINT('Ctrl Pts',(-0.048790709571801,0.146475657227381,
0.756230540755664));
#15065=CARTESIAN_POINT('Ctrl Pts',(-0.000344588961360588,0.146589539830481,
0.753584210876561));
#15066=CARTESIAN_POINT('Ctrl Pts',(0.0481015316490792,0.14670342243358,
0.750937880997459));
#15067=CARTESIAN_POINT('Ctrl Pts',(0.0966096924455767,0.120425158610167,
0.748291551118357));
#15068=CARTESIAN_POINT('Ctrl Pts',(0.122976945064223,0.0797827231418903,
0.745645221239255));
#15069=CARTESIAN_POINT('Ctrl Pts',(0.149344197682869,0.0391402876736125,
0.742998891360154));
#15070=CARTESIAN_POINT('Ctrl Pts',(0.153570542123663,-0.01586631943953,
0.740352561481052));
#15071=CARTESIAN_POINT('Ctrl Pts',(0.133721514043982,-0.0600597087159893,
0.73770623160195));
#15072=CARTESIAN_POINT('Ctrl Pts',(0.113872485964301,-0.104253097992448,
0.735059901722848));
#15073=CARTESIAN_POINT('Ctrl Pts',(0.0699480853641458,-0.137633269432224,
0.732413571843746));
#15074=CARTESIAN_POINT('Ctrl Pts',(0.0220532014503509,-0.144921593405036,
0.729767241964644));
#15075=CARTESIAN_POINT('Ctrl Pts',(-0.0258416824634434,-0.152209917377848,
0.727120912085542));
#15076=CARTESIAN_POINT('Ctrl Pts',(-0.0777070496908773,-0.133406393883698,
0.724474582206441));
#15077=CARTESIAN_POINT('Ctrl Pts',(-0.109803305666473,-0.0971176914572187,
0.721828252327339));
#15078=CARTESIAN_POINT('Ctrl Pts',(-0.133101311474982,-0.0707764758164216,
0.71990733641299));
#15079=CARTESIAN_POINT('Ctrl Pts',(-0.14598295937539,-0.0352223077304616,
0.71798642049864));
#15080=CARTESIAN_POINT('Ctrl Pts',(-0.146290249280603,0.000131112932912382,
0.716065504584291));
#15081=CARTESIAN_POINT('Ctrl Pts',(-0.146307221518699,0.000133045872591754,
0.708934495415711));
#15082=CARTESIAN_POINT('Ctrl Pts',(-0.145987367488279,-0.0358102803178394,
0.710888040627207));
#15083=CARTESIAN_POINT('Ctrl Pts',(-0.132622002370819,-0.0719663061161047,
0.712841585838703));
#15084=CARTESIAN_POINT('Ctrl Pts',(-0.1086007072861,-0.0984612847532928,
0.7147951310502));
#15085=CARTESIAN_POINT('Ctrl Pts',(-0.0760477256663158,-0.134366532557423,
0.71744252042446));
#15086=CARTESIAN_POINT('Ctrl Pts',(-0.0239252288417074,-0.152529358077047,
0.720089909798719));
#15087=CARTESIAN_POINT('Ctrl Pts',(0.0238920022682765,-0.144630254255197,
0.722737299172979));
#15088=CARTESIAN_POINT('Ctrl Pts',(0.071709233378259,-0.136731150433346,
0.725384688547239));
#15089=CARTESIAN_POINT('Ctrl Pts',(0.115221198773618,-0.102770117270024,
0.7280320779215));
#15090=CARTESIAN_POINT('Ctrl Pts',(0.134497183226257,-0.058303052428779,
0.730679467295759));
#15091=CARTESIAN_POINT('Ctrl Pts',(0.153773167678896,-0.0138359875875333,
0.733326856670019));
#15092=CARTESIAN_POINT('Ctrl Pts',(0.148813171188813,0.0411371089316358,
0.735974246044279));
#15093=CARTESIAN_POINT('Ctrl Pts',(0.121889126928366,0.0814357351225549,
0.738621635418539));
#15094=CARTESIAN_POINT('Ctrl Pts',(0.0949650826679194,0.121734361313473,
0.741269024792799));
#15095=CARTESIAN_POINT('Ctrl Pts',(0.0460769906371109,0.147358517176143,
0.74391641416706));
#15096=CARTESIAN_POINT('Ctrl Pts',(-0.00238189178169058,0.146571023090686,
0.74656380354132));
#15097=CARTESIAN_POINT('Ctrl Pts',(-0.0508407742004934,0.14578352900523,
0.74921119291558));
#15098=CARTESIAN_POINT('Ctrl Pts',(-0.0988704470072894,0.118584384971644,
0.751858582289839));
#15099=CARTESIAN_POINT('Ctrl Pts',(-0.124470852918682,0.0774321960944291,
0.754505971664099));
#15100=CARTESIAN_POINT('Ctrl Pts',(-0.138745545153454,0.0544858868428234,
0.75598214624797));
#15101=CARTESIAN_POINT('Ctrl Pts',(-0.146046671909043,0.027201385339783,
0.757458320831841));
#15102=CARTESIAN_POINT('Ctrl Pts',(-0.14612241379348,-4.54149644099216E-5,
0.758934495415711));
#15103=CARTESIAN_POINT('Origin',(0.,0.,0.));
#15104=CARTESIAN_POINT('',(-0.146495788566881,-0.000101744904923998,0.816065504584291));
#15105=CARTESIAN_POINT('',(-0.146473871348434,-0.000110945968026819,0.808934495415711));
#15106=CARTESIAN_POINT('',(-0.14635,-1.79227059055215E-17,0.));
#15107=CARTESIAN_POINT('Ctrl Pts',(-0.146495788566881,-0.000101744904923998,
0.816065504584291));
#15108=CARTESIAN_POINT('Ctrl Pts',(-0.14616118452328,0.0421270051992108,
0.813762715835428));
#15109=CARTESIAN_POINT('Ctrl Pts',(-0.126905337350145,0.0846218946815527,
0.811459927086565));
#15110=CARTESIAN_POINT('Ctrl Pts',(-0.0947343415465314,0.111866064832055,
0.809157138337701));
#15111=CARTESIAN_POINT('Ctrl Pts',(-0.0577639214515077,0.143174651664521,
0.806510808458599));
#15112=CARTESIAN_POINT('Ctrl Pts',(-0.00373742343573488,0.154342745753647,
0.803864478579497));
#15113=CARTESIAN_POINT('Ctrl Pts',(0.0426163743729279,0.140258534729872,
0.801218148700395));
#15114=CARTESIAN_POINT('Ctrl Pts',(0.0889701721815907,0.126174323706097,
0.798571818821294));
#15115=CARTESIAN_POINT('Ctrl Pts',(0.127651269783143,0.0868378075694234,
0.795925488942192));
#15116=CARTESIAN_POINT('Ctrl Pts',(0.140954720244851,0.040253928627653,
0.79327915906309));
#15117=CARTESIAN_POINT('Ctrl Pts',(0.154258170706558,-0.00632995031411615,
0.790632829183988));
#15118=CARTESIAN_POINT('Ctrl Pts',(0.14218397402842,-0.060161192060982,
0.787986499304886));
#15119=CARTESIAN_POINT('Ctrl Pts',(0.110258679990485,-0.0966003903512828,
0.785340169425784));
#15120=CARTESIAN_POINT('Ctrl Pts',(0.0783333859525485,-0.133039588641585,
0.782693839546682));
#15121=CARTESIAN_POINT('Ctrl Pts',(0.0265569945548152,-0.152086743475322,
0.780047509667581));
#15122=CARTESIAN_POINT('Ctrl Pts',(-0.021371625274328,-0.14502367242074,
0.777401179788479));
#15123=CARTESIAN_POINT('Ctrl Pts',(-0.0693002451034712,-0.137960601366157,
0.774754849909377));
#15124=CARTESIAN_POINT('Ctrl Pts',(-0.113381093364023,-0.104787304423254,
0.772108520030274));
#15125=CARTESIAN_POINT('Ctrl Pts',(-0.133437672293631,-0.0606877215103841,
0.769462190151172));
#15126=CARTESIAN_POINT('Ctrl Pts',(-0.1420188514214,-0.0418197768941368,
0.768329961628878));
#15127=CARTESIAN_POINT('Ctrl Pts',(-0.146202281842484,-0.0209517273285418,
0.767197733106584));
#15128=CARTESIAN_POINT('Ctrl Pts',(-0.1461301977291,-5.61458017395017E-5,
0.766065504584291));
#15129=CARTESIAN_POINT('Ctrl Pts',(-0.14612241379348,-4.54149644099216E-5,
0.758934495415711));
#15130=CARTESIAN_POINT('Ctrl Pts',(-0.146182508321779,-0.0216633562673834,
0.760105710206101));
#15131=CARTESIAN_POINT('Ctrl Pts',(-0.141694203021096,-0.0432575645610501,
0.76127692499649));
#15132=CARTESIAN_POINT('Ctrl Pts',(-0.132531725405586,-0.0626424774360703,
0.76244813978688));
#15133=CARTESIAN_POINT('Ctrl Pts',(-0.111821052965107,-0.106459728368519,
0.76509552916114));
#15134=CARTESIAN_POINT('Ctrl Pts',(-0.067228569068158,-0.138988996512573,
0.767742918535399));
#15135=CARTESIAN_POINT('Ctrl Pts',(-0.0191799219195066,-0.145330206128911,
0.770390307909659));
#15136=CARTESIAN_POINT('Ctrl Pts',(0.0288687252291434,-0.151671415745249,
0.773037697283919));
#15137=CARTESIAN_POINT('Ctrl Pts',(0.080373535629496,-0.131824566833873,
0.77568508665818));
#15138=CARTESIAN_POINT('Ctrl Pts',(0.111742660473083,-0.0948805356683208,
0.77833247603244));
#15139=CARTESIAN_POINT('Ctrl Pts',(0.14311178531667,-0.0579365045027684,
0.7809798654067));
#15140=CARTESIAN_POINT('Ctrl Pts',(0.154345224603492,-0.00389529108304171,
0.783627254780959));
#15141=CARTESIAN_POINT('Ctrl Pts',(0.140297486112651,0.0424894529122293,
0.786274644155219));
#15142=CARTESIAN_POINT('Ctrl Pts',(0.126249747621811,0.0888741969075009,
0.788922033529479));
#15143=CARTESIAN_POINT('Ctrl Pts',(0.0869208313533056,0.127602471478316,
0.79156942290374));
#15144=CARTESIAN_POINT('Ctrl Pts',(0.0403254011646538,0.140934737517831,
0.794216812278));
#15145=CARTESIAN_POINT('Ctrl Pts',(-0.00627002902399674,0.154267003557346,
0.79686420165226));
#15146=CARTESIAN_POINT('Ctrl Pts',(-0.0601319731327944,0.142203261065564,
0.799511591026519));
#15147=CARTESIAN_POINT('Ctrl Pts',(-0.0965888940360299,0.110269323781398,
0.802158980400779));
#15148=CARTESIAN_POINT('Ctrl Pts',(-0.127690529151203,0.0830262752573849,
0.804417485405756));
#15149=CARTESIAN_POINT('Ctrl Pts',(-0.146124951115714,0.0413218847513699,
0.806675990410734));
#15150=CARTESIAN_POINT('Ctrl Pts',(-0.146473871348434,-0.000110945968026819,
0.808934495415711));
#15151=CARTESIAN_POINT('Origin',(0.,0.,0.));
#15152=CARTESIAN_POINT('',(-0.146444331750498,0.000119944961782359,0.866065504584291));
#15153=CARTESIAN_POINT('',(-0.146471560192382,0.00011177640072981,0.858934495415711));
#15154=CARTESIAN_POINT('',(-0.14635,-1.79227059055215E-17,0.));
#15155=CARTESIAN_POINT('Ctrl Pts',(-0.146444331750498,0.000119944961782359,
0.866065504584291));
#15156=CARTESIAN_POINT('Ctrl Pts',(-0.146516681599632,0.00829054204730037,
0.865620358322474));
#15157=CARTESIAN_POINT('Ctrl Pts',(-0.145891801779796,0.0164500693154795,
0.865175212060658));
#15158=CARTESIAN_POINT('Ctrl Pts',(-0.14453063157077,0.0244848619971339,
0.864730065798841));
#15159=CARTESIAN_POINT('Ctrl Pts',(-0.136438672357208,0.0722505376181754,
0.862083735919739));
#15160=CARTESIAN_POINT('Ctrl Pts',(-0.102325254887189,0.115607931012472,
0.859437406040638));
#15161=CARTESIAN_POINT('Ctrl Pts',(-0.0578046270350215,0.134711681091902,
0.856791076161536));
#15162=CARTESIAN_POINT('Ctrl Pts',(-0.0132839991828526,0.153815431171333,
0.854144746282434));
#15163=CARTESIAN_POINT('Ctrl Pts',(0.0416438390514653,0.148665537935894,
0.851498416403331));
#15164=CARTESIAN_POINT('Ctrl Pts',(0.081837551941475,0.121619188541491,
0.848852086524229));
#15165=CARTESIAN_POINT('Ctrl Pts',(0.122031264831484,0.0945728391470885,
0.846205756645128));
#15166=CARTESIAN_POINT('Ctrl Pts',(0.147490852377186,0.0456300335937214,
0.843559426766026));
#15167=CARTESIAN_POINT('Ctrl Pts',(0.146563060809277,-0.0028073360113171,
0.840913096886925));
#15168=CARTESIAN_POINT('Ctrl Pts',(0.145635269241369,-0.0512447056163556,
0.838266767007823));
#15169=CARTESIAN_POINT('Ctrl Pts',(0.118320098559852,-0.0991766392730661,
0.835620437128721));
#15170=CARTESIAN_POINT('Ctrl Pts',(0.0771201321287374,-0.124663936845065,
0.832974107249619));
#15171=CARTESIAN_POINT('Ctrl Pts',(0.035920165697623,-0.150151234417064,
0.830327777370517));
#15172=CARTESIAN_POINT('Ctrl Pts',(-0.0191645964830881,-0.153193895904352,
0.827681447491415));
#15173=CARTESIAN_POINT('Ctrl Pts',(-0.0629209921278279,-0.132399247274726,
0.825035117612313));
#15174=CARTESIAN_POINT('Ctrl Pts',(-0.106677387772568,-0.111604598645101,
0.822388787733211));
#15175=CARTESIAN_POINT('Ctrl Pts',(-0.139105416881337,-0.0669726398985626,
0.819742457854109));
#15176=CARTESIAN_POINT('Ctrl Pts',(-0.145362260348583,-0.0189321207373897,
0.817096127975007));
#15177=CARTESIAN_POINT('Ctrl Pts',(-0.146174510965348,-0.0126955988357878,
0.816752586844768));
#15178=CARTESIAN_POINT('Ctrl Pts',(-0.146545706411658,-0.00640163348415362,
0.81640904571453));
#15179=CARTESIAN_POINT('Ctrl Pts',(-0.146495788566881,-0.000101744904923998,
0.816065504584291));
#15180=CARTESIAN_POINT('Ctrl Pts',(-0.146473871348434,-0.000110945968026819,
0.808934495415711));
#15181=CARTESIAN_POINT('Ctrl Pts',(-0.146533950748007,-0.00724512552769256,
0.809323379784994));
#15182=CARTESIAN_POINT('Ctrl Pts',(-0.146057826922151,-0.0143712538186879,
0.809712264154277));
#15183=CARTESIAN_POINT('Ctrl Pts',(-0.145017839345608,-0.0214141189368497,
0.81010114852356));
#15184=CARTESIAN_POINT('Ctrl Pts',(-0.137937966054276,-0.0693594922943736,
0.81274853789782));
#15185=CARTESIAN_POINT('Ctrl Pts',(-0.104726321773939,-0.113446106932874,
0.81539592727208));
#15186=CARTESIAN_POINT('Ctrl Pts',(-0.0605955455659204,-0.133480028752914,
0.818043316646339));
#15187=CARTESIAN_POINT('Ctrl Pts',(-0.0164647693578984,-0.153513950572954,
0.820690706020599));
#15188=CARTESIAN_POINT('Ctrl Pts',(0.0385851387778066,-0.149495179574532,
0.823338095394859));
#15189=CARTESIAN_POINT('Ctrl Pts',(0.0793384931690736,-0.12326451930694,
0.825985484769119));
#15190=CARTESIAN_POINT('Ctrl Pts',(0.120091847560339,-0.0970338590393495,
0.828632874143379));
#15191=CARTESIAN_POINT('Ctrl Pts',(0.146548648207165,-0.0485913095025905,
0.83128026351764));
#15192=CARTESIAN_POINT('Ctrl Pts',(0.146590321408106,-0.000126046730599388,
0.833927652891899));
#15193=CARTESIAN_POINT('Ctrl Pts',(0.146631994609047,0.0483392160413931,
0.836575042266159));
#15194=CARTESIAN_POINT('Ctrl Pts',(0.120258540364101,0.0968271920486179,
0.839222431640419));
#15195=CARTESIAN_POINT('Ctrl Pts',(0.0795503554414038,0.123127897600245,
0.841869821014679));
#15196=CARTESIAN_POINT('Ctrl Pts',(0.0388421705187073,0.149428603151872,
0.844517210388939));
#15197=CARTESIAN_POINT('Ctrl Pts',(-0.0162007450817403,0.153542038247903,
0.8471645997632));
#15198=CARTESIAN_POINT('Ctrl Pts',(-0.0603659086281491,0.133584038319734,
0.84981198913746));
#15199=CARTESIAN_POINT('Ctrl Pts',(-0.104531072174558,0.113626038391565,
0.85245937851172));
#15200=CARTESIAN_POINT('Ctrl Pts',(-0.137818483666928,0.0695966034391962,
0.855106767885979));
#15201=CARTESIAN_POINT('Ctrl Pts',(-0.144980798768897,0.0216634763286692,
0.857754157260239));
#15202=CARTESIAN_POINT('Ctrl Pts',(-0.146045237806912,0.0145398171508471,
0.858147603312063));
#15203=CARTESIAN_POINT('Ctrl Pts',(-0.146532654486068,0.00732993751956911,
0.858541049363887));
#15204=CARTESIAN_POINT('Ctrl Pts',(-0.146471560192382,0.00011177640072981,
0.858934495415711));
#15205=CARTESIAN_POINT('Origin',(0.,0.,0.));
#15206=CARTESIAN_POINT('',(-0.146114231148477,2.69008449349656E-5,0.916065504584291));
#15207=CARTESIAN_POINT('',(-0.146121644853617,4.41067432152685E-5,0.908934495415711));
#15208=CARTESIAN_POINT('',(-0.14635,-1.79227059055215E-17,0.));
#15209=CARTESIAN_POINT('Ctrl Pts',(-0.146114231148477,2.69008449349656E-5,
0.916065504584291));
#15210=CARTESIAN_POINT('Ctrl Pts',(-0.146151635159142,0.0228038459942234,
0.914831670930419));
#15211=CARTESIAN_POINT('Ctrl Pts',(-0.141147538069067,0.0455652341090756,
0.913597837276548));
#15212=CARTESIAN_POINT('Ctrl Pts',(-0.131015765267123,0.0657531838068269,
0.912364003622676));
#15213=CARTESIAN_POINT('Ctrl Pts',(-0.109285110563454,0.109052354902802,
0.909717673743574));
#15214=CARTESIAN_POINT('Ctrl Pts',(-0.0639662294071284,0.140513248471977,
0.907071343864472));
#15215=CARTESIAN_POINT('Ctrl Pts',(-0.015802286694576,0.145735718560985,
0.90442501398537));
#15216=CARTESIAN_POINT('Ctrl Pts',(0.0323616560179757,0.150958188649994,
0.901778684106268));
#15217=CARTESIAN_POINT('Ctrl Pts',(0.0833706602867547,0.129942235258839,
0.899132354227166));
#15218=CARTESIAN_POINT('Ctrl Pts',(0.113877102345416,0.0923071908936453,
0.896486024348064));
#15219=CARTESIAN_POINT('Ctrl Pts',(0.144383544404078,0.0546721465284523,
0.893839694468962));
#15220=CARTESIAN_POINT('Ctrl Pts',(0.15438742425262,0.000418011189221586,
0.891193364589861));
#15221=CARTESIAN_POINT('Ctrl Pts',(0.139309808695705,-0.0456222438118789,
0.888547034710759));
#15222=CARTESIAN_POINT('Ctrl Pts',(0.124232193138789,-0.0916624988129813,
0.885900704831657));
#15223=CARTESIAN_POINT('Ctrl Pts',(0.0840730821764119,-0.129488873475953,
0.883254374952555));
#15224=CARTESIAN_POINT('Ctrl Pts',(0.0372139327097935,-0.141787641004198,
0.880608045073453));
#15225=CARTESIAN_POINT('Ctrl Pts',(-0.00964521675682358,-0.154086408532443,
0.877961715194351));
#15226=CARTESIAN_POINT('Ctrl Pts',(-0.0632044047276821,-0.140857568925962,
0.875315385315249));
#15227=CARTESIAN_POINT('Ctrl Pts',(-0.0989487482345592,-0.108156170198829,
0.872669055436147));
#15228=CARTESIAN_POINT('Ctrl Pts',(-0.128680439645858,-0.0809555616469925,
0.870467871818862));
#15229=CARTESIAN_POINT('Ctrl Pts',(-0.146086572253705,-0.0402824710322022,
0.868266688201576));
#15230=CARTESIAN_POINT('Ctrl Pts',(-0.146444331750498,0.000119944961782359,
0.866065504584291));
#15231=CARTESIAN_POINT('Ctrl Pts',(-0.146471560192382,0.00011177640072981,
0.858934495415711));
#15232=CARTESIAN_POINT('Ctrl Pts',(-0.146121567926216,-0.0412390669452651,
0.861188438738147));
#15233=CARTESIAN_POINT('Ctrl Pts',(-0.127770397964496,-0.0828616943330661,
0.863442382060584));
#15234=CARTESIAN_POINT('Ctrl Pts',(-0.096778382793969,-0.110103055552942,
0.86569632538302));
#15235=CARTESIAN_POINT('Ctrl Pts',(-0.0603764330055066,-0.142099641055337,
0.86834371475728));
#15236=CARTESIAN_POINT('Ctrl Pts',(-0.00653531471701479,-0.154255992791443,
0.870991104131539));
#15237=CARTESIAN_POINT('Ctrl Pts',(0.040082974241256,-0.14100387723139,
0.873638493505799));
#15238=CARTESIAN_POINT('Ctrl Pts',(0.0867012631995282,-0.127751761671338,
0.876285882880059));
#15239=CARTESIAN_POINT('Ctrl Pts',(0.12609672282758,-0.0890911788151255,
0.878933272254319));
#15240=CARTESIAN_POINT('Ctrl Pts',(0.140224208991091,-0.042730661487191,
0.88158066162858));
#15241=CARTESIAN_POINT('Ctrl Pts',(0.154351695154603,0.00362985584074295,
0.88422805100284));
#15242=CARTESIAN_POINT('Ctrl Pts',(0.143211207853577,0.057690307640398,
0.886875440377099));
#15243=CARTESIAN_POINT('Ctrl Pts',(0.111905662524754,0.09468823006692,0.889522829751359));
#15244=CARTESIAN_POINT('Ctrl Pts',(0.0806001171959318,0.131686152493442,
0.892170219125619));
#15245=CARTESIAN_POINT('Ctrl Pts',(0.0291295138393125,0.15162154554683,
0.894817608499879));
#15246=CARTESIAN_POINT('Ctrl Pts',(-0.0189299673197759,0.145362975188259,
0.897464997874139));
#15247=CARTESIAN_POINT('Ctrl Pts',(-0.0669894484788628,0.139104404829688,
0.9001123872484));
#15248=CARTESIAN_POINT('Ctrl Pts',(-0.11163780744042,0.10665187105916,0.902759776622659));
#15249=CARTESIAN_POINT('Ctrl Pts',(-0.132423802349956,0.0628703013313112,
0.905407165996919));
#15250=CARTESIAN_POINT('Ctrl Pts',(-0.141655418982822,0.043425734493323,
0.90658294246985));
#15251=CARTESIAN_POINT('Ctrl Pts',(-0.146180218154578,0.0217465313827003,
0.907758718942781));
#15252=CARTESIAN_POINT('Ctrl Pts',(-0.146121644853617,4.41067432152685E-5,
0.908934495415711));
#15253=CARTESIAN_POINT('Origin',(0.,0.,0.));
#15254=CARTESIAN_POINT('',(-0.146345621585321,-0.000133809880645736,0.966065504584291));
#15255=CARTESIAN_POINT('',(-0.146309694201085,-0.000133223314395004,0.958934495415711));
#15256=CARTESIAN_POINT('',(-0.14635,-1.79227059055215E-17,0.));
#15257=CARTESIAN_POINT('Ctrl Pts',(-0.146345621585321,-0.000133809880645736,
0.966065504584291));
#15258=CARTESIAN_POINT('Ctrl Pts',(-0.146004672532387,0.0370537288701324,
0.964042983538364));
#15259=CARTESIAN_POINT('Ctrl Pts',(-0.131578083002406,0.0744765756810296,
0.962020462492437));
#15260=CARTESIAN_POINT('Ctrl Pts',(-0.106003654037246,0.101251356830495,
0.959997941446511));
#15261=CARTESIAN_POINT('Ctrl Pts',(-0.0725412702228666,0.136284319036219,
0.957351611567409));
#15262=CARTESIAN_POINT('Ctrl Pts',(-0.0199938687303381,0.153087872523943,
0.954705281688306));
#15263=CARTESIAN_POINT('Ctrl Pts',(0.0275867780614433,0.143970766496025,
0.952058951809204));
#15264=CARTESIAN_POINT('Ctrl Pts',(0.0751674248532248,0.134853660468108,
0.949412621930102));
#15265=CARTESIAN_POINT('Ctrl Pts',(0.11778131694426,0.0998158949245492,
0.946766292051));
#15266=CARTESIAN_POINT('Ctrl Pts',(0.135923405490256,0.0548948063954655,
0.944119962171899));
#15267=CARTESIAN_POINT('Ctrl Pts',(0.154065494036253,0.0099737178663825,
0.941473632292797));
#15268=CARTESIAN_POINT('Ctrl Pts',(0.147735779037212,-0.0448306936482241,
0.938827302413695));
#15269=CARTESIAN_POINT('Ctrl Pts',(0.119831470632095,-0.0844335867733556,
0.936180972534593));
#15270=CARTESIAN_POINT('Ctrl Pts',(0.0919271622269763,-0.124036479898489,
0.933534642655491));
#15271=CARTESIAN_POINT('Ctrl Pts',(0.0424482604157787,-0.148437854634144,
0.93088831277639));
#15272=CARTESIAN_POINT('Ctrl Pts',(-0.00595796300272124,-0.146468817862788,
0.928241982897288));
#15273=CARTESIAN_POINT('Ctrl Pts',(-0.0543641864212212,-0.144499781091432,
0.925595653018186));
#15274=CARTESIAN_POINT('Ctrl Pts',(-0.101697731447024,-0.116160332813065,
0.922949323139084));
#15275=CARTESIAN_POINT('Ctrl Pts',(-0.126293289834417,-0.0744218843624929,
0.920302993259982));
#15276=CARTESIAN_POINT('Ctrl Pts',(-0.139421333187579,-0.052143709087005,
0.918890497034752));
#15277=CARTESIAN_POINT('Ctrl Pts',(-0.146071410932229,-0.0260482098028304,
0.917478000809521));
#15278=CARTESIAN_POINT('Ctrl Pts',(-0.146114231148477,2.69008449349656E-5,
0.916065504584291));
#15279=CARTESIAN_POINT('Ctrl Pts',(-0.146121644853617,4.41067432152685E-5,
0.908934495415711));
#15280=CARTESIAN_POINT('Ctrl Pts',(-0.146048333958771,-0.027118852224649,
0.910406108317041));
#15281=CARTESIAN_POINT('Ctrl Pts',(-0.138795050353101,-0.0543181883240968,
0.91187772121837));
#15282=CARTESIAN_POINT('Ctrl Pts',(-0.124603830013468,-0.0772180274565794,
0.9133493341197));
#15283=CARTESIAN_POINT('Ctrl Pts',(-0.0990742319099257,-0.118414180831446,
0.91599672349396));
#15284=CARTESIAN_POINT('Ctrl Pts',(-0.0510914048453256,-0.145695881896007,
0.91864411286822));
#15285=CARTESIAN_POINT('Ctrl Pts',(-0.00263394834681351,-0.146566710184873,
0.92129150224248));
#15286=CARTESIAN_POINT('Ctrl Pts',(0.0458235081516972,-0.147437538473739,
0.92393889161674));
#15287=CARTESIAN_POINT('Ctrl Pts',(0.0947555940841207,-0.121897493986912,
0.926586280990999));
#15288=CARTESIAN_POINT('Ctrl Pts',(0.121748900601314,-0.0816452290135895,
0.929233670365259));
#15289=CARTESIAN_POINT('Ctrl Pts',(0.148742207118509,-0.0413929640402651,
0.931881059739519));
#15290=CARTESIAN_POINT('Ctrl Pts',(0.153796734220472,0.0135715214195569,
0.93452844911378));
#15291=CARTESIAN_POINT('Ctrl Pts',(0.134597248858856,0.0580716696672091,
0.93717583848804));
#15292=CARTESIAN_POINT('Ctrl Pts',(0.115397763497239,0.102571817914861,
0.9398232278623));
#15293=CARTESIAN_POINT('Ctrl Pts',(0.0719442656720451,0.136607628950342,
0.942470617236559));
#15294=CARTESIAN_POINT('Ctrl Pts',(0.0241406894609324,0.144588953003544,
0.945118006610819));
#15295=CARTESIAN_POINT('Ctrl Pts',(-0.023662886750181,0.152570277056746,
0.947765395985079));
#15296=CARTESIAN_POINT('Ctrl Pts',(-0.0758165413472122,0.134497114127667,
0.950412785359339));
#15297=CARTESIAN_POINT('Ctrl Pts',(-0.108431221550465,0.0986479012011113,
0.953060174733599));
#15298=CARTESIAN_POINT('Ctrl Pts',(-0.132554242808212,0.0721325001574252,
0.955018281627637));
#15299=CARTESIAN_POINT('Ctrl Pts',(-0.145988218858404,0.0358924841874147,
0.956976388521674));
#15300=CARTESIAN_POINT('Ctrl Pts',(-0.146309694201085,-0.000133223314395004,
0.958934495415711));
#15301=CARTESIAN_POINT('Origin',(0.,0.,0.));
#15302=CARTESIAN_POINT('',(-0.146565171121453,5.44893591410845E-5,1.01606550458429));
#15303=CARTESIAN_POINT('',(-0.146582076026177,3.15354312248815E-5,1.00893449541571));
#15304=CARTESIAN_POINT('',(-0.14635,-1.79227059055215E-17,0.));
#15305=CARTESIAN_POINT('Ctrl Pts',(-0.146565171121453,5.44893591410845E-5,
1.01606550458429));
#15306=CARTESIAN_POINT('Ctrl Pts',(-0.146579596851449,0.00307427920823236,
1.01590062602541));
#15307=CARTESIAN_POINT('Ctrl Pts',(-0.146494352296349,0.00609323927190738,
1.01573574746653));
#15308=CARTESIAN_POINT('Ctrl Pts',(-0.146306854564556,0.00910583530985269,
1.01557086890765));
#15309=CARTESIAN_POINT('Ctrl Pts',(-0.143297482980539,0.0574585317612167,
1.01292453902855));
#15310=CARTESIAN_POINT('Ctrl Pts',(-0.11394685994478,0.104171803331984,
1.01027820914945));
#15311=CARTESIAN_POINT('Ctrl Pts',(-0.0716892273871119,0.127864250695428,
1.00763187927034));
#15312=CARTESIAN_POINT('Ctrl Pts',(-0.0294315948294418,0.151556698058874,
1.00498554939124));
#15313=CARTESIAN_POINT('Ctrl Pts',(0.0257330472501378,0.152228321214993,
1.00233921951214));
#15314=CARTESIAN_POINT('Ctrl Pts',(0.0685549742796134,0.129571707678744,
0.999692889633039));
#15315=CARTESIAN_POINT('Ctrl Pts',(0.111376901309088,0.106915094142495,
0.997046559753937));
#15316=CARTESIAN_POINT('Ctrl Pts',(0.141856113288459,0.0609302439138786,
0.994400229874835));
#15317=CARTESIAN_POINT('Ctrl Pts',(0.146041795372579,0.0126651464112397,
0.991753899995733));
#15318=CARTESIAN_POINT('Ctrl Pts',(0.150227477456699,-0.0355999510913994,
0.989107570116631));
#15319=CARTESIAN_POINT('Ctrl Pts',(0.128119629645567,-0.0861452958680607,
0.986461240237529));
#15320=CARTESIAN_POINT('Ctrl Pts',(0.0898373616998479,-0.115835488396583,
0.983814910358427));
#15321=CARTESIAN_POINT('Ctrl Pts',(0.051555093754129,-0.145525680925106,
0.981168580479325));
#15322=CARTESIAN_POINT('Ctrl Pts',(-0.00290159432617693,-0.154360721205491,
0.978522250600224));
#15323=CARTESIAN_POINT('Ctrl Pts',(-0.0486070196525971,-0.138296672301818,
0.975875920721122));
#15324=CARTESIAN_POINT('Ctrl Pts',(-0.0943124449790173,-0.122232623398145,
0.97322959084202));
#15325=CARTESIAN_POINT('Ctrl Pts',(-0.131266607551552,-0.081269485310415,
0.970583260962917));
#15326=CARTESIAN_POINT('Ctrl Pts',(-0.142555005769704,-0.0341567308046872,
0.967936931083816));
#15327=CARTESIAN_POINT('Ctrl Pts',(-0.145215975052668,-0.0230510282813687,
0.967313122250641));
#15328=CARTESIAN_POINT('Ctrl Pts',(-0.146450780951306,-0.0116036114945705,
0.966689313417466));
#15329=CARTESIAN_POINT('Ctrl Pts',(-0.146345621585321,-0.000133809880645736,
0.966065504584291));
#15330=CARTESIAN_POINT('Ctrl Pts',(-0.146309694201085,-0.000133223314395004,
0.958934495415711));
#15331=CARTESIAN_POINT('Ctrl Pts',(-0.146422858258782,-0.0128148032088542,
0.959623777895933));
#15332=CARTESIAN_POINT('Ctrl Pts',(-0.14491119500038,-0.0254698272036438,
0.960313060376156));
#15333=CARTESIAN_POINT('Ctrl Pts',(-0.141668994059001,-0.037664762585484,
0.961002342856379));
#15334=CARTESIAN_POINT('Ctrl Pts',(-0.129216380554811,-0.0845029505214961,
0.963649732230639));
#15335=CARTESIAN_POINT('Ctrl Pts',(-0.0912354477369537,-0.12455406346949,
0.966297121604899));
#15336=CARTESIAN_POINT('Ctrl Pts',(-0.0451234138007503,-0.1394726343957,
0.968944510979159));
#15337=CARTESIAN_POINT('Ctrl Pts',(0.00098862013545236,-0.154391205321909,
0.97159190035342));
#15338=CARTESIAN_POINT('Ctrl Pts',(0.055231755190001,-0.144177234226336,
0.974239289727679));
#15339=CARTESIAN_POINT('Ctrl Pts',(0.0927598492034174,-0.113509244531313,
0.976886679101939));
#15340=CARTESIAN_POINT('Ctrl Pts',(0.130287943216833,-0.0828412548362905,
0.979534068476199));
#15341=CARTESIAN_POINT('Ctrl Pts',(0.151100996189117,-0.0317192465418168,
0.982181457850459));
#15342=CARTESIAN_POINT('Ctrl Pts',(0.145665560755875,0.0164402745715088,
0.984828847224719));
#15343=CARTESIAN_POINT('Ctrl Pts',(0.140230125322634,0.0645997956848379,
0.987476236598979));
#15344=CARTESIAN_POINT('Ctrl Pts',(0.108546201483865,0.109796829617019,
0.990123625973239));
#15345=CARTESIAN_POINT('Ctrl Pts',(0.0651266538643092,0.131328813193254,
0.992771015347499));
#15346=CARTESIAN_POINT('Ctrl Pts',(0.0217071062447581,0.152860796769488,
0.995418404721759));
#15347=CARTESIAN_POINT('Ctrl Pts',(-0.0334480651555777,0.15072772998978,
0.998065794096019));
#15348=CARTESIAN_POINT('Ctrl Pts',(-0.0750749586823209,0.125906667008376,
1.00071318347028));
#15349=CARTESIAN_POINT('Ctrl Pts',(-0.116701852209067,0.101085604026969,
1.00336057284454));
#15350=CARTESIAN_POINT('Ctrl Pts',(-0.144800467862219,0.053576544843864,
1.0060079622188));
#15351=CARTESIAN_POINT('Ctrl Pts',(-0.146500196332402,0.00514107896046776,
1.00865535159306));
#15352=CARTESIAN_POINT('Ctrl Pts',(-0.146559936783033,0.00343871495990628,
1.00874839953394));
#15353=CARTESIAN_POINT('Ctrl Pts',(-0.146587066279139,0.00173520655478852,
1.00884144747483));
#15354=CARTESIAN_POINT('Ctrl Pts',(-0.146582076026177,3.15354312248815E-5,
1.00893449541571));
#15355=CARTESIAN_POINT('Origin',(0.,0.,0.));
#15356=CARTESIAN_POINT('',(-0.146184049129756,9.96948043307314E-5,1.06606550458429));
#15357=CARTESIAN_POINT('',(-0.146216477546812,0.000114345603752017,1.05893449541571));
#15358=CARTESIAN_POINT('',(-0.14635,-1.79227059055215E-17,0.));
#15359=CARTESIAN_POINT('Ctrl Pts',(-0.146184049129756,9.96948043307314E-5,
1.06606550458429));
#15360=CARTESIAN_POINT('Ctrl Pts',(-0.146294264763128,0.0176817746259609,
1.06511193863336));
#15361=CARTESIAN_POINT('Ctrl Pts',(-0.143360807533043,0.0352283113603788,
1.06415837268242));
#15362=CARTESIAN_POINT('Ctrl Pts',(-0.13721959397524,0.0515693218739058,
1.06320480673148));
#15363=CARTESIAN_POINT('Ctrl Pts',(-0.120176538991979,0.0969187854681546,
1.06055847685238));
#15364=CARTESIAN_POINT('Ctrl Pts',(-0.0784283132238915,0.132983650068601,
1.05791214697328));
#15365=CARTESIAN_POINT('Ctrl Pts',(-0.0310837364199337,0.143256459747686,
1.05526581709418));
#15366=CARTESIAN_POINT('Ctrl Pts',(0.0162608403840241,0.153529269426771,
1.05261948721508));
#15367=CARTESIAN_POINT('Ctrl Pts',(0.0692017682238519,0.138010024184496,
1.04997315733597));
#15368=CARTESIAN_POINT('Ctrl Pts',(0.103507151520239,0.103802126728842,
1.04732682745687));
#15369=CARTESIAN_POINT('Ctrl Pts',(0.137812534816628,0.0695942292731864,
1.04468049757777));
#15370=CARTESIAN_POINT('Ctrl Pts',(0.153482373569574,0.01669767960415,1.04203416769867));
#15371=CARTESIAN_POINT('Ctrl Pts',(0.143344336052008,-0.0306759392859165,
1.03938783781957));
#15372=CARTESIAN_POINT('Ctrl Pts',(0.133206298534443,-0.0780495581759789,
1.03674150794047));
#15373=CARTESIAN_POINT('Ctrl Pts',(0.0972603847463712,-0.119900246287072,
1.03409517806136));
#15374=CARTESIAN_POINT('Ctrl Pts',(0.0519596049571008,-0.137072285243832,
1.03144884818226));
#15375=CARTESIAN_POINT('Ctrl Pts',(0.00665882516783032,-0.154244324200591,
1.02880251830316));
#15376=CARTESIAN_POINT('Ctrl Pts',(-0.0479968206226384,-0.146737714003016,
1.02615618842406));
#15377=CARTESIAN_POINT('Ctrl Pts',(-0.0869905834517384,-0.11798834823825,
1.02350985854496));
#15378=CARTESIAN_POINT('Ctrl Pts',(-0.123554854979944,-0.0910302005802824,
1.02102840722473));
#15379=CARTESIAN_POINT('Ctrl Pts',(-0.146348061346918,-0.0453938791777224,
1.01854695590451));
#15380=CARTESIAN_POINT('Ctrl Pts',(-0.146565171121453,5.44893591410845E-5,
1.01606550458429));
#15381=CARTESIAN_POINT('Ctrl Pts',(-0.146582076026177,3.15354312248815E-5,
1.00893449541571));
#15382=CARTESIAN_POINT('Ctrl Pts',(-0.146445084172466,-0.0467374494427972,
1.01148883684909));
#15383=CARTESIAN_POINT('Ctrl Pts',(-0.122102455869861,-0.0936290599181376,
1.01404317828246));
#15384=CARTESIAN_POINT('Ctrl Pts',(-0.0837162036049941,-0.120334265578335,
1.01659751971584));
#15385=CARTESIAN_POINT('Ctrl Pts',(-0.0439316411201867,-0.14801227165006,
1.0192449090901));
#15386=CARTESIAN_POINT('Ctrl Pts',(0.0109383251366414,-0.154006411209824,
1.02189229846436));
#15387=CARTESIAN_POINT('Ctrl Pts',(0.0557604321169594,-0.135571060438576,
1.02453968783862));
#15388=CARTESIAN_POINT('Ctrl Pts',(0.100582539097277,-0.11713570966733,
1.02718707721288));
#15389=CARTESIAN_POINT('Ctrl Pts',(0.135356786801084,-0.0742708685650716,
1.02983446658714));
#15390=CARTESIAN_POINT('Ctrl Pts',(0.144154783532934,-0.0266108361928598,
1.0324818559614));
#15391=CARTESIAN_POINT('Ctrl Pts',(0.152952780264784,0.0210491961793507,
1.03512924533566));
#15392=CARTESIAN_POINT('Ctrl Pts',(0.135774526024679,0.0735044198215165,
1.03777663470992));
#15393=CARTESIAN_POINT('Ctrl Pts',(0.100488543649143,0.106727647840587,
1.04042402408418));
#15394=CARTESIAN_POINT('Ctrl Pts',(0.0652025612736062,0.139950875859659,
1.04307141345844));
#15395=CARTESIAN_POINT('Ctrl Pts',(0.0118088507626404,0.153942108255635,
1.0457188028327));
#15396=CARTESIAN_POINT('Ctrl Pts',(-0.0352355257975899,0.142292641904202,
1.04836619220696));
#15397=CARTESIAN_POINT('Ctrl Pts',(-0.0822799023578202,0.130643175552769,
1.05101358158122));
#15398=CARTESIAN_POINT('Ctrl Pts',(-0.122974944967313,0.0933530104539243,
1.05366097095548));
#15399=CARTESIAN_POINT('Ctrl Pts',(-0.138680233730631,0.0475029577050484,
1.05630836032974));
#15400=CARTESIAN_POINT('Ctrl Pts',(-0.143873300563147,0.0323423075707214,
1.05718373869173));
#15401=CARTESIAN_POINT('Ctrl Pts',(-0.146334133026589,0.0162457690968458,
1.05805911705372));
#15402=CARTESIAN_POINT('Ctrl Pts',(-0.146216477546812,0.000114345603752017,
1.05893449541571));
#15403=CARTESIAN_POINT('Origin',(0.,0.,0.));
#15404=CARTESIAN_POINT('',(-0.146204073634541,-0.000109175101205505,1.11606550458429));
#15405=CARTESIAN_POINT('',(-0.146170555016798,-9.22629125885076E-5,1.10893449541571));
#15406=CARTESIAN_POINT('',(-0.14635,-1.79227059055215E-17,0.));
#15407=CARTESIAN_POINT('Ctrl Pts',(-0.146204073634541,-0.000109175101205505,
1.11606550458429));
#15408=CARTESIAN_POINT('Ctrl Pts',(-0.145981599624502,0.032003853555373,
1.1143232512413));
#15409=CARTESIAN_POINT('Ctrl Pts',(-0.135565881201595,0.0642480963468658,
1.11258099789831));
#15410=CARTESIAN_POINT('Ctrl Pts',(-0.11609067353381,0.0895073597405865,
1.11083874455532));
#15411=CARTESIAN_POINT('Ctrl Pts',(-0.0865095427755784,0.127873963375947,
1.10819241467622));
#15412=CARTESIAN_POINT('Ctrl Pts',(-0.0360273159486943,0.150125560802435,
1.10554608479712));
#15413=CARTESIAN_POINT('Ctrl Pts',(0.0122494975033169,0.14607724579886,
1.10289975491801));
#15414=CARTESIAN_POINT('Ctrl Pts',(0.0605263109553308,0.142028930795284,
1.10025342503891));
#15415=CARTESIAN_POINT('Ctrl Pts',(0.10659771103247,0.111680703361642,1.09760709515981));
#15416=CARTESIAN_POINT('Ctrl Pts',(0.129376093089052,0.0689234246557527,
1.09496076528071));
#15417=CARTESIAN_POINT('Ctrl Pts',(0.152154475145634,0.0261661459498645,
1.09231443540161));
#15418=CARTESIAN_POINT('Ctrl Pts',(0.151639839181659,-0.0290001840282729,
1.0896681055225));
#15419=CARTESIAN_POINT('Ctrl Pts',(0.128067742174483,-0.0713250681289163,
1.0870217756434));
#15420=CARTESIAN_POINT('Ctrl Pts',(0.104495645167307,-0.11364995222956,
1.0843754457643));
#15421=CARTESIAN_POINT('Ctrl Pts',(0.0578660871169326,-0.143133390452712,
1.0817291158852));
#15422=CARTESIAN_POINT('Ctrl Pts',(0.00952215035475689,-0.146280349267719,
1.0790827860061));
#15423=CARTESIAN_POINT('Ctrl Pts',(-0.0388217864074202,-0.149427308082725,
1.07643645612699));
#15424=CARTESIAN_POINT('Ctrl Pts',(-0.0888801018813974,-0.126237787489585,
1.07379012624789));
#15425=CARTESIAN_POINT('Ctrl Pts',(-0.117740317519168,-0.0873259958989869,
1.07114379636879));
#15426=CARTESIAN_POINT('Ctrl Pts',(-0.136201180005177,-0.0624354946409797,
1.06945103244062));
#15427=CARTESIAN_POINT('Ctrl Pts',(-0.145988395071105,-0.0311118962502767,
1.06775826851246));
#15428=CARTESIAN_POINT('Ctrl Pts',(-0.146184049129756,9.96948043307314E-5,
1.06606550458429));
#15429=CARTESIAN_POINT('Ctrl Pts',(-0.146216477546812,0.000114345603752017,
1.05893449541571));
#15430=CARTESIAN_POINT('Ctrl Pts',(-0.145978309898544,-0.0325401742182177,
1.06070650642798));
#15431=CARTESIAN_POINT('Ctrl Pts',(-0.135174246449945,-0.06533764273189,
1.06247851744025));
#15432=CARTESIAN_POINT('Ctrl Pts',(-0.115079600404687,-0.0908043159161929,
1.06425052845252));
#15433=CARTESIAN_POINT('Ctrl Pts',(-0.0850581433982766,-0.128851596389654,
1.06689791782678));
#15434=CARTESIAN_POINT('Ctrl Pts',(-0.0342996944683099,-0.150536216937668,
1.06954530720104));
#15435=CARTESIAN_POINT('Ctrl Pts',(0.0139457694684962,-0.145925507476389,
1.0721926965753));
#15436=CARTESIAN_POINT('Ctrl Pts',(0.0621912334052997,-0.14131479801511,
1.07484008594956));
#15437=CARTESIAN_POINT('Ctrl Pts',(0.107923712348941,-0.110408758544542,
1.07748747532382));
#15438=CARTESIAN_POINT('Ctrl Pts',(0.1301953818052,-0.0673639426912374,
1.08013486469808));
#15439=CARTESIAN_POINT('Ctrl Pts',(0.15246705126146,-0.024319126837932,
1.08278225407234));
#15440=CARTESIAN_POINT('Ctrl Pts',(0.151277911230334,0.0308644653981125,
1.0854296434466));
#15441=CARTESIAN_POINT('Ctrl Pts',(0.127172648928576,0.0729099141598672,
1.08807703282086));
#15442=CARTESIAN_POINT('Ctrl Pts',(0.103067386626818,0.114955362921624,
1.09072442219512));
#15443=CARTESIAN_POINT('Ctrl Pts',(0.0560460020544268,0.143862668209093,
1.09337181156938));
#15444=CARTESIAN_POINT('Ctrl Pts',(0.00764670469074742,0.146390799320458,
1.09601920094364));
#15445=CARTESIAN_POINT('Ctrl Pts',(-0.0407525926729279,0.148918930431823,
1.0986665903179));
#15446=CARTESIAN_POINT('Ctrl Pts',(-0.0905298028278899,0.125067887367091,
1.10131397969216));
#15447=CARTESIAN_POINT('Ctrl Pts',(-0.11888440661962,0.0857626730052823,
1.10396136906642));
#15448=CARTESIAN_POINT('Ctrl Pts',(-0.136639133674055,0.0611510311732957,
1.10561907784952));
#15449=CARTESIAN_POINT('Ctrl Pts',(-0.145994366384503,0.0304800321277272,
1.10727678663261));
#15450=CARTESIAN_POINT('Ctrl Pts',(-0.146170555016798,-9.22629125885076E-5,
1.10893449541571));
#15451=CARTESIAN_POINT('Origin',(0.,0.,0.));
#15452=CARTESIAN_POINT('',(-0.146577386142569,-3.88073511912723E-5,1.16606550458429));
#15453=CARTESIAN_POINT('',(-0.146552328192774,-6.73160170860698E-5,1.15893449541571));
#15454=CARTESIAN_POINT('',(-0.14635,-1.79227059055215E-17,0.));
#15455=CARTESIAN_POINT('Ctrl Pts',(-0.146577386142569,-3.88073511912723E-5,
1.16606550458429));
#15456=CARTESIAN_POINT('Ctrl Pts',(-0.146413350709018,0.0463056768050285,
1.16353456384924));
#15457=CARTESIAN_POINT('Ctrl Pts',(-0.122574225104448,0.0927954474992645,
1.1610036231142));
#15458=CARTESIAN_POINT('Ctrl Pts',(-0.0847742546295189,0.119590709008994,
1.15847268237915));
#15459=CARTESIAN_POINT('Ctrl Pts',(-0.0452509303920754,0.147607604138013,
1.15582635250005));
#15460=CARTESIAN_POINT('Ctrl Pts',(0.00953524646069181,0.154093252855687,
1.15318002262095));
#15461=CARTESIAN_POINT('Ctrl Pts',(0.0545077808453859,0.136079071706768,
1.15053369274185));
#15462=CARTESIAN_POINT('Ctrl Pts',(0.0994803152300801,0.118064890557849,
1.14788736286275));
#15463=CARTESIAN_POINT('Ctrl Pts',(0.134639207146701,0.0755508795423365,
1.14524103298364));
#15464=CARTESIAN_POINT('Ctrl Pts',(0.14389167861853,0.027996370364851,1.14259470310454));
#15465=CARTESIAN_POINT('Ctrl Pts',(0.15314415009036,-0.0195581388126345,
1.13994837322544));
#15466=CARTESIAN_POINT('Ctrl Pts',(0.136490201117397,-0.0721531461520931,
1.13730204334634));
#15467=CARTESIAN_POINT('Ctrl Pts',(0.101552606157185,-0.105715089329518,
1.13465571346724));
#15468=CARTESIAN_POINT('Ctrl Pts',(0.0666150111969725,-0.139277032506943,
1.13200938358813));
#15469=CARTESIAN_POINT('Ctrl Pts',(0.0133937702495101,-0.153805911522335,
1.12936305370903));
#15470=CARTESIAN_POINT('Ctrl Pts',(-0.033750917386428,-0.142651629870951,
1.12671672382993));
#15471=CARTESIAN_POINT('Ctrl Pts',(-0.0808956050223675,-0.131497348219567,
1.12407039395083));
#15472=CARTESIAN_POINT('Ctrl Pts',(-0.121963739346782,-0.094659905901407,
1.12142406407173));
#15473=CARTESIAN_POINT('Ctrl Pts',(-0.1381577891642,-0.0490003798202082,
1.11877773419262));
#15474=CARTESIAN_POINT('Ctrl Pts',(-0.143690228857438,-0.0334015285560649,
1.11787365765651));
#15475=CARTESIAN_POINT('Ctrl Pts',(-0.146319518115206,-0.0167730178360648,
1.1169695811204));
#15476=CARTESIAN_POINT('Ctrl Pts',(-0.146204073634541,-0.000109175101205505,
1.11606550458429));
#15477=CARTESIAN_POINT('Ctrl Pts',(-0.146170555016798,-9.22629125885076E-5,
1.10893449541571));
#15478=CARTESIAN_POINT('Ctrl Pts',(-0.146275742653821,-0.0183444476975235,
1.10992417600687));
#15479=CARTESIAN_POINT('Ctrl Pts',(-0.143109248288425,-0.0365614514641733,
1.11091385659804));
#15480=CARTESIAN_POINT('Ctrl Pts',(-0.136505188007283,-0.0534328725168923,
1.1119035371892));
#15481=CARTESIAN_POINT('Ctrl Pts',(-0.118839368174718,-0.0985638180183679,
1.11455092656346));
#15482=CARTESIAN_POINT('Ctrl Pts',(-0.0765757310810901,-0.134066323362434,
1.11719831593772));
#15483=CARTESIAN_POINT('Ctrl Pts',(-0.0290731934694857,-0.143678417446031,
1.11984570531198));
#15484=CARTESIAN_POINT('Ctrl Pts',(0.01842934414212,-0.153290511529629,
1.12249309468624));
#15485=CARTESIAN_POINT('Ctrl Pts',(0.071170782271703,-0.137012194352758,
1.1251404840605));
#15486=CARTESIAN_POINT('Ctrl Pts',(0.10499283308901,-0.102299771349957,
1.12778787343476));
#15487=CARTESIAN_POINT('Ctrl Pts',(0.138814883906317,-0.0675873483471558,
1.13043526280902));
#15488=CARTESIAN_POINT('Ctrl Pts',(0.153717547411349,-0.0144408195184256,
1.13308265218328));
#15489=CARTESIAN_POINT('Ctrl Pts',(0.142874638214406,0.0327959749574983,
1.13573004155754));
#15490=CARTESIAN_POINT('Ctrl Pts',(0.132031729017462,0.0800327694334235,
1.1383774309318));
#15491=CARTESIAN_POINT('Ctrl Pts',(0.0954432471185425,0.121359829556542,
1.14102482030606));
#15492=CARTESIAN_POINT('Ctrl Pts',(0.0498685966661331,0.137847238945365,
1.14367220968032));
#15493=CARTESIAN_POINT('Ctrl Pts',(0.00429394621372511,0.154334648334189,
1.14631959905458));
#15494=CARTESIAN_POINT('Ctrl Pts',(-0.0502668727921719,0.145982406988718,
1.14896698842884));
#15495=CARTESIAN_POINT('Ctrl Pts',(-0.0888222026239048,0.116616270474356,
1.1516143778031));
#15496=CARTESIAN_POINT('Ctrl Pts',(-0.124357782404925,0.0895501633622979,
1.1540544170073));
#15497=CARTESIAN_POINT('Ctrl Pts',(-0.146296868742479,0.0446329749882746,
1.15649445621151));
#15498=CARTESIAN_POINT('Ctrl Pts',(-0.146552328192774,-6.73160170860698E-5,
1.15893449541571));
#15499=CARTESIAN_POINT('Origin',(0.,0.,0.));
#15500=CARTESIAN_POINT('',(-0.146318311025392,0.000133437649768732,1.21606550458429));
#15501=CARTESIAN_POINT('',(-0.146373054956946,0.000132657382717961,1.20893449541571));
#15502=CARTESIAN_POINT('',(-0.14635,-1.79227059055215E-17,0.));
#15503=CARTESIAN_POINT('Ctrl Pts',(-0.146318311025392,0.000133437649768732,
1.21606550458429));
#15504=CARTESIAN_POINT('Ctrl Pts',(-0.146429658069886,0.0125190846592594,
1.21539220633629));
#15505=CARTESIAN_POINT('Ctrl Pts',(-0.144988168643405,0.0248791929292086,
1.21471890808829));
#15506=CARTESIAN_POINT('Ctrl Pts',(-0.141892968227885,0.0368102906365087,
1.21404560984029));
#15507=CARTESIAN_POINT('Ctrl Pts',(-0.129727599662405,0.083704249513052,
1.21139927996119));
#15508=CARTESIAN_POINT('Ctrl Pts',(-0.0920156607298113,0.123970842060419,
1.20875295008209));
#15509=CARTESIAN_POINT('Ctrl Pts',(-0.0460184991925076,0.139179415364965,
1.20610662020299));
#15510=CARTESIAN_POINT('Ctrl Pts',(-2.13376552038805E-5,0.15438798866951,
1.20346029032389));
#15511=CARTESIAN_POINT('Ctrl Pts',(0.0542610464868107,0.144538542731236,
1.20081396044478));
#15512=CARTESIAN_POINT('Ctrl Pts',(0.091982751999895,0.114139323915075,
1.19816763056568));
#15513=CARTESIAN_POINT('Ctrl Pts',(0.129704457512977,0.0837401050989159,
1.19552130068658));
#15514=CARTESIAN_POINT('Ctrl Pts',(0.150865484397133,0.0327911134048729,
1.19287497080748));
#15515=CARTESIAN_POINT('Ctrl Pts',(0.145780097726084,-0.0153874961003253,
1.19022864092838));
#15516=CARTESIAN_POINT('Ctrl Pts',(0.140694711055036,-0.063566105605525,
1.18758231104927));
#15517=CARTESIAN_POINT('Ctrl Pts',(0.109362910828785,-0.108974332921877,
1.18493598117017));
#15518=CARTESIAN_POINT('Ctrl Pts',(0.0661257549466402,-0.130828118009858,
1.18228965129107));
#15519=CARTESIAN_POINT('Ctrl Pts',(0.0228885990644955,-0.152681903097838,
1.17964332141197));
#15520=CARTESIAN_POINT('Ctrl Pts',(-0.0322539124735426,-0.150981245957443,
1.17699699153287));
#15521=CARTESIAN_POINT('Ctrl Pts',(-0.0740621845924981,-0.126504564117865,
1.17435066165376));
#15522=CARTESIAN_POINT('Ctrl Pts',(-0.115870456711455,-0.102027882278287,
1.17170433177466));
#15523=CARTESIAN_POINT('Ctrl Pts',(-0.144344489411329,-0.0547751757395235,
1.16905800189556));
#15524=CARTESIAN_POINT('Ctrl Pts',(-0.146451269950206,-0.00637475169995868,
1.16641167201646));
#15525=CARTESIAN_POINT('Ctrl Pts',(-0.146543132875163,-0.00426432565444621,
1.1662962828724));
#15526=CARTESIAN_POINT('Ctrl Pts',(-0.146584864748453,-0.00215171749738942,
1.16618089372835));
#15527=CARTESIAN_POINT('Ctrl Pts',(-0.146577386142569,-3.88073511912723E-5,
1.16606550458429));
#15528=CARTESIAN_POINT('Ctrl Pts',(-0.146552328192774,-6.73160170860698E-5,
1.15893449541571));
#15529=CARTESIAN_POINT('Ctrl Pts',(-0.146574036680232,-0.00386586684592084,
1.15914184558577));
#15530=CARTESIAN_POINT('Ctrl Pts',(-0.1464391612665,-0.00766285139452399,
1.15934919575582));
#15531=CARTESIAN_POINT('Ctrl Pts',(-0.146142739258869,-0.0114471821958193,
1.15955654592588));
#15532=CARTESIAN_POINT('Ctrl Pts',(-0.142358105404532,-0.0597644666683822,
1.16220393530014));
#15533=CARTESIAN_POINT('Ctrl Pts',(-0.112238997038288,-0.106019003930254,
1.1648513246744));
#15534=CARTESIAN_POINT('Ctrl Pts',(-0.0695815129186611,-0.129023839960917,
1.16749871404866));
#15535=CARTESIAN_POINT('Ctrl Pts',(-0.026924028799035,-0.15202867599158,
1.17014610342292));
#15536=CARTESIAN_POINT('Ctrl Pts',(0.0282718310739737,-0.151783810791035,
1.17279349279718));
#15537=CARTESIAN_POINT('Ctrl Pts',(0.0707235276354612,-0.128401405199111,
1.17544088217144));
#15538=CARTESIAN_POINT('Ctrl Pts',(0.11317522419695,-0.105018999607187,
1.1780882715457));
#15539=CARTESIAN_POINT('Ctrl Pts',(0.142882757446916,-0.0584990536238821,
1.18073566091996));
#15540=CARTESIAN_POINT('Ctrl Pts',(0.146238551171451,-0.0101500920973681,
1.18338305029422));
#15541=CARTESIAN_POINT('Ctrl Pts',(0.149594344895986,0.0381988694291446,
1.18603043966848));
#15542=CARTESIAN_POINT('Ctrl Pts',(0.12659839909509,0.0883768464988665,
1.18867782904274));
#15543=CARTESIAN_POINT('Ctrl Pts',(0.0877840381772113,0.117399748124142,
1.191325218417));
#15544=CARTESIAN_POINT('Ctrl Pts',(0.0489696772593311,0.146422649749419,
1.19397260779126));
#15545=CARTESIAN_POINT('Ctrl Pts',(-0.00566309877553352,0.154290475930249,
1.19661999716552));
#15546=CARTESIAN_POINT('Ctrl Pts',(-0.0510896721842483,0.137399358129564,
1.19926738653978));
#15547=CARTESIAN_POINT('Ctrl Pts',(-0.0965162455929618,0.12050824032888,
1.20191477591404));
#15548=CARTESIAN_POINT('Ctrl Pts',(-0.132736616375526,0.0788581785466829,
1.2045621652883));
#15549=CARTESIAN_POINT('Ctrl Pts',(-0.143159994183491,0.0315270405159292,
1.20720955466256));
#15550=CARTESIAN_POINT('Ctrl Pts',(-0.145423823013163,0.021247302336111,
1.20778453491361));
#15551=CARTESIAN_POINT('Ctrl Pts',(-0.146470795531708,0.0106995851133921,
1.20835951516466));
#15552=CARTESIAN_POINT('Ctrl Pts',(-0.146373054956946,0.000132657382717961,
1.20893449541571));
#15553=CARTESIAN_POINT('Origin',(0.,0.,0.));
#15554=CARTESIAN_POINT('',(-0.146120596765396,-4.14129048147555E-5,1.26606550458429));
#15555=CARTESIAN_POINT('',(-0.146109918970638,-1.0198006988139E-5,1.25893449541571));
#15556=CARTESIAN_POINT('',(-0.14635,-1.79227059055215E-17,0.));
#15557=CARTESIAN_POINT('Ctrl Pts',(-0.146120596765396,-4.14129048147555E-5,
1.26606550458429));
#15558=CARTESIAN_POINT('Ctrl Pts',(-0.14605219935785,0.0269443530192317,
1.26460351894424));
#15559=CARTESIAN_POINT('Ctrl Pts',(-0.138898723445843,0.053963836666407,
1.26314153330418));
#15560=CARTESIAN_POINT('Ctrl Pts',(-0.124882896249422,0.0767650581554474,
1.26167954766413));
#15561=CARTESIAN_POINT('Ctrl Pts',(-0.0995129464537159,0.118037388097231,
1.25903321778503));
#15562=CARTESIAN_POINT('Ctrl Pts',(-0.051658938874944,0.145488850208621,
1.25638688790592));
#15563=CARTESIAN_POINT('Ctrl Pts',(-0.00322440565727106,0.146554478394238,
1.25374055802682));
#15564=CARTESIAN_POINT('Ctrl Pts',(0.0452101275604033,0.147620106579856,
1.25109422814772));
#15565=CARTESIAN_POINT('Ctrl Pts',(0.0942251864169787,0.122299900839699,
1.24844789826862));
#15566=CARTESIAN_POINT('Ctrl Pts',(0.121385807331354,0.0821833176976391,
1.24580156838952));
#15567=CARTESIAN_POINT('Ctrl Pts',(0.148546428245729,0.0420667345555804,
1.24315523851041));
#15568=CARTESIAN_POINT('Ctrl Pts',(0.153852611217905,-0.0128462259883804,
1.24050890863131));
#15569=CARTESIAN_POINT('Ctrl Pts',(0.134875632820701,-0.0574210379606392,
1.23786257875221));
#15570=CARTESIAN_POINT('Ctrl Pts',(0.115898654423498,-0.101995849932898,
1.23521624887311));
#15571=CARTESIAN_POINT('Ctrl Pts',(0.0726385146569148,-0.136232513333455,
1.23256991899401));
#15572=CARTESIAN_POINT('Ctrl Pts',(0.0248960600935515,-0.144460368686643,
1.2299235891149));
#15573=CARTESIAN_POINT('Ctrl Pts',(-0.0228463944698117,-0.152688224039831,
1.2272772592358));
#15574=CARTESIAN_POINT('Ctrl Pts',(-0.0750711638299551,-0.134907271345651,
1.2246309293567));
#15575=CARTESIAN_POINT('Ctrl Pts',(-0.107874149410843,-0.0992561323957017,
1.2219845994776));
#15576=CARTESIAN_POINT('Ctrl Pts',(-0.132331163880887,-0.072675612185966,
1.2200115678465));
#15577=CARTESIAN_POINT('Ctrl Pts',(-0.145992019903337,-0.0361614337449312,
1.21803853621539));
#15578=CARTESIAN_POINT('Ctrl Pts',(-0.146318311025392,0.000133437649768732,
1.21606550458429));
#15579=CARTESIAN_POINT('Ctrl Pts',(-0.146373054956946,0.000132657382717961,
1.20893449541571));
#15580=CARTESIAN_POINT('Ctrl Pts',(-0.146020767276673,-0.0379538636644633,
1.21100690453892));
#15581=CARTESIAN_POINT('Ctrl Pts',(-0.130797424420382,-0.0762899498869128,
1.21307931366213));
#15582=CARTESIAN_POINT('Ctrl Pts',(-0.104081054125652,-0.103227285106232,
1.21515172278534));
#15583=CARTESIAN_POINT('Ctrl Pts',(-0.0699523514264828,-0.137638258418326,
1.2177991121596));
#15584=CARTESIAN_POINT('Ctrl Pts',(-0.0170685611947798,-0.153447990763203,
1.22044650153386));
#15585=CARTESIAN_POINT('Ctrl Pts',(0.0303468241642401,-0.143414812629152,
1.22309389090812));
#15586=CARTESIAN_POINT('Ctrl Pts',(0.0777622095232573,-0.133381634495101,
1.22574128028238));
#15587=CARTESIAN_POINT('Ctrl Pts',(0.119709190009594,-0.0975055458821257,
1.22838866965664));
#15588=CARTESIAN_POINT('Ctrl Pts',(0.136973893871985,-0.052219638220276,
1.2310360590309));
#15589=CARTESIAN_POINT('Ctrl Pts',(0.154238597734379,-0.00693373055842239,
1.23368344840516));
#15590=CARTESIAN_POINT('Ctrl Pts',(0.146821024972825,0.0477619961523044,
1.23633083777942));
#15591=CARTESIAN_POINT('Ctrl Pts',(0.118118804930222,0.0868140895256425,
1.23897822715368));
#15592=CARTESIAN_POINT('Ctrl Pts',(0.0894165848876198,0.125866182898978,
1.24162561652794));
#15593=CARTESIAN_POINT('Ctrl Pts',(0.0394297175639698,0.149274642934924,
1.2442730059022));
#15594=CARTESIAN_POINT('Ctrl Pts',(-0.00894524413350711,0.146317192515786,
1.24692039527646));
#15595=CARTESIAN_POINT('Ctrl Pts',(-0.0573202058309854,0.143359742096648,
1.24956778465072));
#15596=CARTESIAN_POINT('Ctrl Pts',(-0.104083261902292,0.114036381222425,
1.25221517402498));
#15597=CARTESIAN_POINT('Ctrl Pts',(-0.127814530591109,0.0717787154251623,
1.25486256339924));
#15598=CARTESIAN_POINT('Ctrl Pts',(-0.139981499518435,0.0501133037087236,
1.2562198740714));
#15599=CARTESIAN_POINT('Ctrl Pts',(-0.146094355379323,0.0250479932723348,
1.25757718474355));
#15600=CARTESIAN_POINT('Ctrl Pts',(-0.146109918970638,-1.0198006988139E-5,
1.25893449541571));
#15601=CARTESIAN_POINT('Origin',(0.,0.,0.));
#15602=CARTESIAN_POINT('',(-0.146470135615938,-0.000111966546850736,1.31606550458429));
#15603=CARTESIAN_POINT('',(-0.146410535958061,-0.000127756381200432,1.30893449541571));
#15604=CARTESIAN_POINT('',(-0.14635,-1.79227059055215E-17,0.));
#15605=CARTESIAN_POINT('Ctrl Pts',(-0.146470135615938,-0.000111966546850736,
1.31606550458429));
#15606=CARTESIAN_POINT('Ctrl Pts',(-0.146120207411574,0.0411799307449602,
1.31381483155218));
#15607=CARTESIAN_POINT('Ctrl Pts',(-0.127827491572984,0.0827431563937987,
1.31156415852007));
#15608=CARTESIAN_POINT('Ctrl Pts',(-0.0969137672218927,0.10998333351997,
1.30931348548796));
#15609=CARTESIAN_POINT('Ctrl Pts',(-0.0605655677022408,0.142012194937238,
1.30666715560886));
#15610=CARTESIAN_POINT('Ctrl Pts',(-0.00676890401288169,0.154239532672684,
1.30402082572976));
#15611=CARTESIAN_POINT('Ctrl Pts',(0.0398526445220406,0.14106870189023,
1.30137449585066));
#15612=CARTESIAN_POINT('Ctrl Pts',(0.0864741930569617,0.127897871107775,
1.29872816597155));
#15613=CARTESIAN_POINT('Ctrl Pts',(0.125920626437448,0.0893288718074177,
1.29608183609245));
#15614=CARTESIAN_POINT('Ctrl Pts',(0.14013669149516,0.0430153417578024,
1.29343550621335));
#15615=CARTESIAN_POINT('Ctrl Pts',(0.154352756552873,-0.00329818829181684,
1.29078917633425));
#15616=CARTESIAN_POINT('Ctrl Pts',(0.143338453287813,-0.0573562490906975,
1.28814284645515));
#15617=CARTESIAN_POINT('Ctrl Pts',(0.112135201594409,-0.0944156157243562,
1.28549651657604));
#15618=CARTESIAN_POINT('Ctrl Pts',(0.0809319499010078,-0.131474982358013,
1.28285018669694));
#15619=CARTESIAN_POINT('Ctrl Pts',(0.0295397497792676,-0.151535654826449,
1.28020385681784));
#15620=CARTESIAN_POINT('Ctrl Pts',(-0.0185183802362589,-0.1454155477333,
1.27755752693874));
#15621=CARTESIAN_POINT('Ctrl Pts',(-0.066576510251784,-0.139295440640151,
1.27491119705964));
#15622=CARTESIAN_POINT('Ctrl Pts',(-0.111300570161094,-0.106994553985419,
1.27226486718053));
#15623=CARTESIAN_POINT('Ctrl Pts',(-0.13221965410943,-0.0632975117719662,
1.26961853730143));
#15624=CARTESIAN_POINT('Ctrl Pts',(-0.141581826511298,-0.0437412423069929,
1.26843419306239));
#15625=CARTESIAN_POINT('Ctrl Pts',(-0.146176005022067,-0.0219023912433209,
1.26724984882334));
#15626=CARTESIAN_POINT('Ctrl Pts',(-0.146120596765396,-4.14129048147555E-5,
1.26606550458429));
#15627=CARTESIAN_POINT('Ctrl Pts',(-0.146109918970638,-1.0198006988139E-5,
1.25893449541571));
#15628=CARTESIAN_POINT('Ctrl Pts',(-0.146124711647138,-0.0238271763493914,
1.26022457411781));
#15629=CARTESIAN_POINT('Ctrl Pts',(-0.140631289159497,-0.0476377233371588,
1.26151465281992));
#15630=CARTESIAN_POINT('Ctrl Pts',(-0.129592576141605,-0.0685164391025303,
1.26280473152202));
#15631=CARTESIAN_POINT('Ctrl Pts',(-0.106939871696956,-0.111361957112663,
1.26545212089628));
#15632=CARTESIAN_POINT('Ctrl Pts',(-0.0609349815013302,-0.141861022412626,
1.26809951027054));
#15633=CARTESIAN_POINT('Ctrl Pts',(-0.0126505083952331,-0.146043496451057,
1.2707468996448));
#15634=CARTESIAN_POINT('Ctrl Pts',(0.0356339647108625,-0.150225970489488,
1.27339428901906));
#15635=CARTESIAN_POINT('Ctrl Pts',(0.0861980207274291,-0.128091853266388,
1.27604167839332));
#15636=CARTESIAN_POINT('Ctrl Pts',(0.11588072467734,-0.0897797074320025,
1.27868906776758));
#15637=CARTESIAN_POINT('Ctrl Pts',(0.145563428627253,-0.0514675615976161,
1.28133645714184));
#15638=CARTESIAN_POINT('Ctrl Pts',(0.154364780510509,0.00302261284805656,
1.2839838465161));
#15639=CARTESIAN_POINT('Ctrl Pts',(0.138253309066183,0.0487315170146188,
1.28663123589036));
#15640=CARTESIAN_POINT('Ctrl Pts',(0.122141837621857,0.0944404211811797,
1.28927862526462));
#15641=CARTESIAN_POINT('Ctrl Pts',(0.0811175428499519,0.131368055068631,
1.29192601463888));
#15642=CARTESIAN_POINT('Ctrl Pts',(0.0339716590485425,0.142599665496764,
1.29457340401314));
#15643=CARTESIAN_POINT('Ctrl Pts',(-0.013174224752867,0.153831275924897,
1.2972207933874));
#15644=CARTESIAN_POINT('Ctrl Pts',(-0.0664416975837803,0.139366862893713,
1.29986818276166));
#15645=CARTESIAN_POINT('Ctrl Pts',(-0.101431520699135,0.105831870563862,
1.30251557213592));
#15646=CARTESIAN_POINT('Ctrl Pts',(-0.129710573305276,0.0787286237393239,
1.30465521322918));
#15647=CARTESIAN_POINT('Ctrl Pts',(-0.146050663974784,0.0391684733249047,
1.30679485432245));
#15648=CARTESIAN_POINT('Ctrl Pts',(-0.146410535958061,-0.000127756381200432,
1.30893449541571));
#15649=CARTESIAN_POINT('Origin',(0.,0.,0.));
#15650=CARTESIAN_POINT('',(-0.146471469669193,0.000111495080380188,1.36606550458429));
#15651=CARTESIAN_POINT('',(-0.146526884620975,8.5711493927648E-5,1.35893449541571));
#15652=CARTESIAN_POINT('',(-0.14635,-1.79227059055215E-17,0.));
#15653=CARTESIAN_POINT('Ctrl Pts',(-0.146471469669193,0.000111495080380188,
1.36606550458429));
#15654=CARTESIAN_POINT('Ctrl Pts',(-0.146532402405025,0.0073220458586883,
1.36567247403923));
#15655=CARTESIAN_POINT('Ctrl Pts',(-0.146045973070864,0.0145243451116175,
1.36527944349416));
#15656=CARTESIAN_POINT('Ctrl Pts',(-0.144983764805735,0.0216407019395156,
1.3648864129491));
#15657=CARTESIAN_POINT('Ctrl Pts',(-0.137831767320671,0.0695561322809842,
1.36224008307));
#15658=CARTESIAN_POINT('Ctrl Pts',(-0.104576727819841,0.113575347233418,
1.3595937531909));
#15659=CARTESIAN_POINT('Ctrl Pts',(-0.060440002550743,0.133550058215342,
1.3569474233118));
#15660=CARTESIAN_POINT('Ctrl Pts',(-0.0163032772816473,0.153524769197265,
1.35430109343269));
#15661=CARTESIAN_POINT('Ctrl Pts',(0.0387151337557165,0.149454976208681,
1.35165476355359));
#15662=CARTESIAN_POINT('Ctrl Pts',(0.0794324390145508,0.123203488242689,
1.34900843367449));
#15663=CARTESIAN_POINT('Ctrl Pts',(0.120149744273387,0.0969520002766962,
1.34636210379539));
#15664=CARTESIAN_POINT('Ctrl Pts',(0.146565943753694,0.048518817333291,
1.34371577391629));
#15665=CARTESIAN_POINT('Ctrl Pts',(0.14658992694451,7.25688577880009E-5,
1.34106944403718));
#15666=CARTESIAN_POINT('Ctrl Pts',(0.146613910135327,-0.0483736796177136,
1.33842311415808));
#15667=CARTESIAN_POINT('Ctrl Pts',(0.120245677036657,-0.0968329936253116,
1.33577678427898));
#15668=CARTESIAN_POINT('Ctrl Pts',(0.0795543829983497,-0.123124782547022,
1.33313045439988));
#15669=CARTESIAN_POINT('Ctrl Pts',(0.0388630889600415,-0.149416571468734,
1.33048412452078));
#15670=CARTESIAN_POINT('Ctrl Pts',(-0.0161512660179049,-0.153540835304554,
1.32783779464168));
#15671=CARTESIAN_POINT('Ctrl Pts',(-0.0603077462478081,-0.133609833714981,
1.32519146476257));
#15672=CARTESIAN_POINT('Ctrl Pts',(-0.10446422647771,-0.113678832125408,
1.32254513488347));
#15673=CARTESIAN_POINT('Ctrl Pts',(-0.137762831959571,-0.0696925651104417,
1.31989880500437));
#15674=CARTESIAN_POINT('Ctrl Pts',(-0.144962267025529,-0.0217842390534145,
1.31725247512527));
#15675=CARTESIAN_POINT('Ctrl Pts',(-0.146038665626028,-0.0146213916011371,
1.31685681827827));
#15676=CARTESIAN_POINT('Ctrl Pts',(-0.146531651210624,-0.00737087161912708,
1.31646116143128));
#15677=CARTESIAN_POINT('Ctrl Pts',(-0.146470135615938,-0.000111966546850736,
1.31606550458429));
#15678=CARTESIAN_POINT('Ctrl Pts',(-0.146410535958061,-0.000127756381200432,
1.30893449541571));
#15679=CARTESIAN_POINT('Ctrl Pts',(-0.146495935505426,-0.00945296197092968,
1.30944224369671));
#15680=CARTESIAN_POINT('Ctrl Pts',(-0.145681427739287,-0.018763305174839,
1.3099499919777));
#15681=CARTESIAN_POINT('Ctrl Pts',(-0.143913007029536,-0.0278887903271487,
1.3104577402587));
#15682=CARTESIAN_POINT('Ctrl Pts',(-0.134692496844786,-0.0754688872597875,
1.31310512963296));
#15683=CARTESIAN_POINT('Ctrl Pts',(-0.0995393030754929,-0.118023509496548,
1.31575251900722));
#15684=CARTESIAN_POINT('Ctrl Pts',(-0.0545553941775042,-0.136060454153345,
1.31839990838148));
#15685=CARTESIAN_POINT('Ctrl Pts',(-0.00957148527951295,-0.154097398810142,
1.32104729775574));
#15686=CARTESIAN_POINT('Ctrl Pts',(0.0452431387471776,-0.14761666588697,
1.32369468713));
#15687=CARTESIAN_POINT('Ctrl Pts',(0.0847805644327026,-0.119586763955155,
1.32634207650426));
#15688=CARTESIAN_POINT('Ctrl Pts',(0.124317990118227,-0.09155686202334,
1.32898946587852));
#15689=CARTESIAN_POINT('Ctrl Pts',(0.148578217462589,-0.041977791082884,
1.33163685525278));
#15690=CARTESIAN_POINT('Ctrl Pts',(0.146448816178573,0.00644068764408242,
1.33428424462704));
#15691=CARTESIAN_POINT('Ctrl Pts',(0.144319414894557,0.0548591663710502,
1.3369316340013));
#15692=CARTESIAN_POINT('Ctrl Pts',(0.115800384982161,0.102117052884526,
1.33957902337556));
#15693=CARTESIAN_POINT('Ctrl Pts',(0.0739549070570988,0.126567807678519,
1.34222641274982));
#15694=CARTESIAN_POINT('Ctrl Pts',(0.0321094291320376,0.151018562472512,
1.34487380212408));
#15695=CARTESIAN_POINT('Ctrl Pts',(-0.0230624968056921,0.152662185547021,
1.34752119149834));
#15696=CARTESIAN_POINT('Ctrl Pts',(-0.0662892946253695,0.1307458130856,
1.3501685808726));
#15697=CARTESIAN_POINT('Ctrl Pts',(-0.109516092445046,0.10882944062418,
1.35281597024686));
#15698=CARTESIAN_POINT('Ctrl Pts',(-0.140797762146673,0.0633530726268328,
1.35546335962112));
#15699=CARTESIAN_POINT('Ctrl Pts',(-0.145805692234247,0.0151472216574969,
1.35811074899538));
#15700=CARTESIAN_POINT('Ctrl Pts',(-0.146325105122407,0.0101474034011793,
1.35838533113549));
#15701=CARTESIAN_POINT('Ctrl Pts',(-0.146561879835735,0.00511822289583405,
1.3586599132756));
#15702=CARTESIAN_POINT('Ctrl Pts',(-0.146526884620975,8.5711493927648E-5,
1.35893449541571));
#15703=CARTESIAN_POINT('Origin',(0.,0.,0.));
#15704=CARTESIAN_POINT('',(-0.146120987371435,4.2191387702159E-5,1.41606550458429));
#15705=CARTESIAN_POINT('',(-0.146148882937928,7.6306569664006E-5,1.40893449541571));
#15706=CARTESIAN_POINT('',(-0.14635,-1.79227059055215E-17,0.));
#15707=CARTESIAN_POINT('Ctrl Pts',(-0.146120987371435,4.2191387702159E-5,
1.41606550458429));
#15708=CARTESIAN_POINT('Ctrl Pts',(-0.146177309023295,0.021854523983563,
1.41488378664717));
#15709=CARTESIAN_POINT('Ctrl Pts',(-0.141604359564088,0.0436444172696427,
1.41370206871005));
#15710=CARTESIAN_POINT('Ctrl Pts',(-0.132282279973341,0.0631665524487371,
1.41252035077294));
#15711=CARTESIAN_POINT('Ctrl Pts',(-0.1114064880593,0.106884268839086,1.40987402089383));
#15712=CARTESIAN_POINT('Ctrl Pts',(-0.0667143915920224,0.139229456738304,
1.40722769101473));
#15713=CARTESIAN_POINT('Ctrl Pts',(-0.0186623352932378,0.145397151366753,
1.40458136113563));
#15714=CARTESIAN_POINT('Ctrl Pts',(0.0293897210055454,0.151564845995202,
1.40193503125653));
#15715=CARTESIAN_POINT('Ctrl Pts',(0.0808017371358351,0.131555047352884,
1.39928870137743));
#15716=CARTESIAN_POINT('Ctrl Pts',(0.112041660826149,0.0945265884816804,
1.39664237149832));
#15717=CARTESIAN_POINT('Ctrl Pts',(0.143281584516463,0.0574981296104763,
1.39399604161922));
#15718=CARTESIAN_POINT('Ctrl Pts',(0.154349415766802,0.00345101051038574,
1.39134971174012));
#15719=CARTESIAN_POINT('Ctrl Pts',(0.140179214932283,-0.0428765696854336,
1.38870338186102));
#15720=CARTESIAN_POINT('Ctrl Pts',(0.126009014097764,-0.089204149881253,
1.38605705198192));
#15721=CARTESIAN_POINT('Ctrl Pts',(0.0866007811783877,-0.127812191172801,
1.38341072210282));
#15722=CARTESIAN_POINT('Ctrl Pts',(0.0399922944706322,-0.14102917638501,
1.38076439222371));
#15723=CARTESIAN_POINT('Ctrl Pts',(-0.00661619223712474,-0.15424616159722,
1.37811806234461));
#15724=CARTESIAN_POINT('Ctrl Pts',(-0.060424932733261,-0.142072090730089,
1.37547173246551));
#15725=CARTESIAN_POINT('Ctrl Pts',(-0.0968048252466797,-0.110079232431271,
1.37282540258641));
#15726=CARTESIAN_POINT('Ctrl Pts',(-0.127781608685608,-0.08283792481198,
1.37057210325237));
#15727=CARTESIAN_POINT('Ctrl Pts',(-0.146122133733866,-0.0412276055847571,
1.36831880391833));
#15728=CARTESIAN_POINT('Ctrl Pts',(-0.146471469669193,0.000111495080380188,
1.36606550458429));
#15729=CARTESIAN_POINT('Ctrl Pts',(-0.146526884620975,8.5711493927648E-5,
1.35893449541571));
#15730=CARTESIAN_POINT('Ctrl Pts',(-0.146224472749943,-0.0434028397118431,
1.36130730264986));
#15731=CARTESIAN_POINT('Ctrl Pts',(-0.125627402569456,-0.0871401285467012,
1.36368010988401));
#15732=CARTESIAN_POINT('Ctrl Pts',(-0.0917490966422633,-0.114327780902106,
1.36605291711816));
#15733=CARTESIAN_POINT('Ctrl Pts',(-0.0539503804891888,-0.144661598551044,
1.36870030649242));
#15734=CARTESIAN_POINT('Ctrl Pts',(0.00038124229047478,-0.154393899907594,
1.37134769586668));
#15735=CARTESIAN_POINT('Ctrl Pts',(0.0463590973565905,-0.139066790892088,
1.37399508524094));
#15736=CARTESIAN_POINT('Ctrl Pts',(0.0923369524227062,-0.123739681876581,
1.3766424746152));
#15737=CARTESIAN_POINT('Ctrl Pts',(0.129961039775272,-0.083353162489017,
1.37928986398946));
#15738=CARTESIAN_POINT('Ctrl Pts',(0.141997595260484,-0.0364063334065561,
1.38193725336372));
#15739=CARTESIAN_POINT('Ctrl Pts',(0.154034150745695,0.0105404956759021,
1.38458464273798));
#15740=CARTESIAN_POINT('Ctrl Pts',(0.140483174363557,0.0640476344532581,
1.38723203211224));
#15741=CARTESIAN_POINT('Ctrl Pts',(0.10755170844225,0.0996060653705087,
1.3898794214865));
#15742=CARTESIAN_POINT('Ctrl Pts',(0.0746202425209409,0.135164496287762,
1.39252681086076));
#15743=CARTESIAN_POINT('Ctrl Pts',(0.0223082870604623,0.152774219344908,
1.39517420023502));
#15744=CARTESIAN_POINT('Ctrl Pts',(-0.025422593472234,0.144369075867769,
1.39782158960928));
#15745=CARTESIAN_POINT('Ctrl Pts',(-0.073153474004929,0.135963932390631,
1.40046897898354));
#15746=CARTESIAN_POINT('Ctrl Pts',(-0.11630327960984,0.101543922379208,
1.4031163683578));
#15747=CARTESIAN_POINT('Ctrl Pts',(-0.135107186188192,0.0568751802851974,
1.40576375773206));
#15748=CARTESIAN_POINT('Ctrl Pts',(-0.142614236437708,0.0390421576584788,
1.40682067029328));
#15749=CARTESIAN_POINT('Ctrl Pts',(-0.14624095998336,0.0195756595648056,
1.40787758285449));
#15750=CARTESIAN_POINT('Ctrl Pts',(-0.146148882937928,7.6306569664006E-5,
1.40893449541571));
#15751=CARTESIAN_POINT('Origin',(0.,0.,0.));
#15752=CARTESIAN_POINT('',(-0.14631473222987,-0.000131398079681141,1.46606550458429));
#15753=CARTESIAN_POINT('',(-0.146248097568756,-0.000123763188177425,1.45893449541571));
#15754=CARTESIAN_POINT('',(-0.14635,-1.79227059055215E-17,0.));
#15755=CARTESIAN_POINT('Ctrl Pts',(-0.14631473222987,-0.000131398079681141,
1.46606550458429));
#15756=CARTESIAN_POINT('Ctrl Pts',(-0.145989697979493,0.0361157155227289,
1.46409509925512));
#15757=CARTESIAN_POINT('Ctrl Pts',(-0.132370868650209,0.0725796635271419,
1.46212469392594));
#15758=CARTESIAN_POINT('Ctrl Pts',(-0.107973319296019,0.0991484059484618,
1.46015428859677));
#15759=CARTESIAN_POINT('Ctrl Pts',(-0.0752064754000165,0.134831245351468,
1.45750795871767));
#15760=CARTESIAN_POINT('Ctrl Pts',(-0.0229974942306327,0.152665588379184,
1.45486162883857));
#15761=CARTESIAN_POINT('Ctrl Pts',(0.0247535192036911,0.144485406820094,
1.45221529895946));
#15762=CARTESIAN_POINT('Ctrl Pts',(0.0725045326380122,0.136305225261004,
1.44956896908036));
#15763=CARTESIAN_POINT('Ctrl Pts',(0.115797578337275,0.102110519115111,
1.44692263920126));
#15764=CARTESIAN_POINT('Ctrl Pts',(0.134818450998255,0.0575543070937695,
1.44427630932216));
#15765=CARTESIAN_POINT('Ctrl Pts',(0.153839323659235,0.0129980950724284,
1.44162997944306));
#15766=CARTESIAN_POINT('Ctrl Pts',(0.148588023281934,-0.0419196228243577,
1.43898364956396));
#15767=CARTESIAN_POINT('Ctrl Pts',(0.121467255745355,-0.082062966762292,
1.43633731968485));
#15768=CARTESIAN_POINT('Ctrl Pts',(0.0943464882087764,-0.122206310700226,
1.43369098980575));
#15769=CARTESIAN_POINT('Ctrl Pts',(0.0453562535129183,-0.147575280679306,
1.43104465992665));
#15770=CARTESIAN_POINT('Ctrl Pts',(-0.00307937473935208,-0.146557666176543,
1.42839833004755));
#15771=CARTESIAN_POINT('Ctrl Pts',(-0.0515150029916225,-0.14554005167378,
1.42575200016845));
#15772=CARTESIAN_POINT('Ctrl Pts',(-0.0993960248003067,-0.118135852689175,
1.42310567028934));
#15773=CARTESIAN_POINT('Ctrl Pts',(-0.124806792024246,-0.0768886307561326,
1.42045934041024));
#15774=CARTESIAN_POINT('Ctrl Pts',(-0.138870387581649,-0.0540603453281256,
1.41899472846826));
#15775=CARTESIAN_POINT('Ctrl Pts',(-0.146051182757901,-0.0269918425378075,
1.41753011652627));
#15776=CARTESIAN_POINT('Ctrl Pts',(-0.146120987371435,4.2191387702159E-5,
1.41606550458429));
#15777=CARTESIAN_POINT('Ctrl Pts',(-0.146148882937928,7.6306569664006E-5,
1.40893449541571));
#15778=CARTESIAN_POINT('Ctrl Pts',(-0.146010322369016,-0.0292669616874671,
1.41052497222875));
#15779=CARTESIAN_POINT('Ctrl Pts',(-0.137450455640384,-0.0586846305953837,
1.4121154490418));
#15780=CARTESIAN_POINT('Ctrl Pts',(-0.121019719714466,-0.0827222215753489,
1.41370592585484));
#15781=CARTESIAN_POINT('Ctrl Pts',(-0.0936703391105966,-0.122733407165291,
1.4163533152291));
#15782=CARTESIAN_POINT('Ctrl Pts',(-0.0445135703510636,-0.147838304168576,
1.41900070460336));
#15783=CARTESIAN_POINT('Ctrl Pts',(0.00393424939099551,-0.146537573651384,
1.42164809397762));
#15784=CARTESIAN_POINT('Ctrl Pts',(0.0523820691330518,-0.145236843134192,
1.42429548335188));
#15785=CARTESIAN_POINT('Ctrl Pts',(0.100120939857634,-0.117530485096527,
1.42694287272614));
#15786=CARTESIAN_POINT('Ctrl Pts',(0.125284029446909,-0.0761094471358441,
1.4295902621004));
#15787=CARTESIAN_POINT('Ctrl Pts',(0.150447119036187,-0.0346884091751576,
1.43223765147466));
#15788=CARTESIAN_POINT('Ctrl Pts',(0.153034427490153,0.020447308708549,
1.43488504084892));
#15789=CARTESIAN_POINT('Ctrl Pts',(0.13186079120536,0.0640427391611241,
1.43753243022318));
#15790=CARTESIAN_POINT('Ctrl Pts',(0.110687154920568,0.107638169613697,
1.44017981959744));
#15791=CARTESIAN_POINT('Ctrl Pts',(0.0657525738970213,0.139693312635139,
1.4428272089717));
#15792=CARTESIAN_POINT('Ctrl Pts',(0.0176394768514684,0.145525221357757,
1.44547459834596));
#15793=CARTESIAN_POINT('Ctrl Pts',(-0.0304736201940859,0.151357130080375,
1.44812198772022));
#15794=CARTESIAN_POINT('Ctrl Pts',(-0.0817652332616461,0.130965804504167,
1.45076937709448));
#15795=CARTESIAN_POINT('Ctrl Pts',(-0.112741325423428,0.0936916042199666,
1.45341676646874));
#15796=CARTESIAN_POINT('Ctrl Pts',(-0.134261605244105,0.0677957870194472,
1.45525600945106));
#15797=CARTESIAN_POINT('Ctrl Pts',(-0.145976367207401,0.0337512577971725,
1.45709525243339));
#15798=CARTESIAN_POINT('Ctrl Pts',(-0.146248097568756,-0.000123763188177425,
1.45893449541571));
#15799=CARTESIAN_POINT('Origin',(0.,0.,-0.0924367114736175));
#15800=CARTESIAN_POINT('',(-0.117746618301147,-0.000105742458702955,1.48256328852638));
#15801=CARTESIAN_POINT('',(-0.117971241274414,-5.28325160115065E-6,1.49243671147361));
#15802=CARTESIAN_POINT('',(-0.117775,2.85464118895969E-14,-0.0924367114736175));
#15803=CARTESIAN_POINT('',(-0.117668597464313,0.00500517689812599,1.532225));
#15804=CARTESIAN_POINT('Ctrl Pts',(-0.117746618301147,-0.000105742458702949,
1.48256328852638));
#15805=CARTESIAN_POINT('Ctrl Pts',(-0.117836347163251,-0.0101121102621826,
1.48323921307631));
#15806=CARTESIAN_POINT('Ctrl Pts',(-0.112089674709738,-0.0591937430214443,
1.48656146750534));
#15807=CARTESIAN_POINT('Ctrl Pts',(-0.0435804807853106,-0.132222740314769,
1.49253005181348));
#15808=CARTESIAN_POINT('Ctrl Pts',(0.0874774386997331,-0.108286040948335,
1.50046904145078));
#15809=CARTESIAN_POINT('Ctrl Pts',(0.138385550162814,0.0147146982980264,
1.50840803108809));
#15810=CARTESIAN_POINT('Ctrl Pts',(0.0627460642121078,0.124368470664037,
1.51634702072539));
#15811=CARTESIAN_POINT('Ctrl Pts',(-0.0706026869052757,0.119928391791904,
1.5242860103627));
#15812=CARTESIAN_POINT('Ctrl Pts',(-0.116004137797729,0.0441355889673283,
1.5295786701209));
#15813=CARTESIAN_POINT('Ctrl Pts',(-0.117668597464313,0.00500517689812487,
1.532225));
#15814=CARTESIAN_POINT('',(-0.0334019664627544,0.1129391839063,1.53222500000001));
#15815=CARTESIAN_POINT('Origin',(0.,0.,1.532225));
#15816=CARTESIAN_POINT('Ctrl Pts',(-0.117971276761593,-5.28420699491729E-6,
1.49243671147361));
#15817=CARTESIAN_POINT('Ctrl Pts',(-0.117971582784674,-0.000385634193345565,
1.49246252744444));
#15818=CARTESIAN_POINT('Ctrl Pts',(-0.117794795258817,-0.0397700451254522,
1.49513573278954));
#15819=CARTESIAN_POINT('Ctrl Pts',(-0.0742871760264013,-0.117748889605885,
1.50045632750888));
#15820=CARTESIAN_POINT('Ctrl Pts',(0.0586284551779338,-0.126233948370975,
1.50839849563167));
#15821=CARTESIAN_POINT('Ctrl Pts',(0.137995068118234,-0.019163470063063,
1.51634066375444));
#15822=CARTESIAN_POINT('Ctrl Pts',(0.0906261803825392,0.105639137646141,
1.52428283187723));
#15823=CARTESIAN_POINT('Ctrl Pts',(0.00417072711528833,0.124051375507138,
1.52957761062575));
#15824=CARTESIAN_POINT('Ctrl Pts',(-0.0334019664627544,0.1129391839063,
1.53222500000001));
#15825=CARTESIAN_POINT('Origin',(0.,0.,-0.0924367114736175));
#15826=CARTESIAN_POINT('',(-0.117590702341447,3.3953472435133E-5,1.43256328852638));
#15827=CARTESIAN_POINT('',(-0.117692994131604,-9.95982882293356E-5,1.44243671147361));
#15828=CARTESIAN_POINT('',(-0.117775,2.85464118895969E-14,-0.0924367114736175));
#15829=CARTESIAN_POINT('Ctrl Pts',(-0.117590702341447,3.39534724351446E-5,
1.43256328852638));
#15830=CARTESIAN_POINT('Ctrl Pts',(-0.117534527156218,-0.0217216553118358,
1.43402790046837));
#15831=CARTESIAN_POINT('Ctrl Pts',(-0.101314495966545,-0.0828641818343832,
1.43813884228945));
#15832=CARTESIAN_POINT('Ctrl Pts',(-0.00292444232197888,-0.139176693688359,
1.44489611398964));
#15833=CARTESIAN_POINT('Ctrl Pts',(0.115350068603298,-0.0779297424218237,
1.45283510362695));
#15834=CARTESIAN_POINT('Ctrl Pts',(0.128028003046829,0.0546551750765237,
1.46077409326425));
#15835=CARTESIAN_POINT('Ctrl Pts',(0.0235079116789307,0.137209630484779,
1.46871308290156));
#15836=CARTESIAN_POINT('Ctrl Pts',(-0.0918059616614023,0.0978189523496558,
1.47597614798894));
#15837=CARTESIAN_POINT('Ctrl Pts',(-0.117485047349053,0.0290640819657798,
1.48059288319721));
#15838=CARTESIAN_POINT('Ctrl Pts',(-0.117746618301147,-0.000105742458702949,
1.48256328852638));
#15839=CARTESIAN_POINT('Ctrl Pts',(-0.117692994131604,-9.9598288229346E-5,
1.44243671147361));
#15840=CARTESIAN_POINT('Ctrl Pts',(-0.117789077779518,-0.0120777797952868,
1.44324485786555));
#15841=CARTESIAN_POINT('Ctrl Pts',(-0.110597905189529,-0.0631824179582176,
1.44670039363175));
#15842=CARTESIAN_POINT('Ctrl Pts',(-0.0368790902657646,-0.134252921254984,
1.45280331877221));
#15843=CARTESIAN_POINT('Ctrl Pts',(0.0928396680879532,-0.103751556080299,
1.46074548689499));
#15844=CARTESIAN_POINT('Ctrl Pts',(0.137511141307062,0.0217950526079239,
1.46868765501776));
#15845=CARTESIAN_POINT('Ctrl Pts',(0.0562018483347667,0.127378648737854,
1.47662982314055));
#15846=CARTESIAN_POINT('Ctrl Pts',(-0.0761502833827582,0.1162998103107,
1.48454617529249));
#15847=CARTESIAN_POINT('Ctrl Pts',(-0.117940200573233,0.0386186906477724,
1.48981513807018));
#15848=CARTESIAN_POINT('Ctrl Pts',(-0.117971276761593,-5.28420699491729E-6,
1.49243671147361));
#15849=CARTESIAN_POINT('Origin',(0.,0.,-0.0924367114736175));
#15850=CARTESIAN_POINT('',(-0.117872752581409,8.97255421561373E-5,1.38256328852638));
#15851=CARTESIAN_POINT('',(-0.117613151267609,6.14076272390171E-5,1.39243671147361));
#15852=CARTESIAN_POINT('',(-0.117775,2.85464118895969E-14,-0.0924367114736175));
#15853=CARTESIAN_POINT('Ctrl Pts',(-0.117872752581409,8.97255421561322E-5,
1.38256328852638));
#15854=CARTESIAN_POINT('Ctrl Pts',(-0.117591624875346,-0.0331778698171688,
1.38481658786042));
#15855=CARTESIAN_POINT('Ctrl Pts',(-0.0854981695600773,-0.105990339321694,
1.38971621707357));
#15856=CARTESIAN_POINT('Ctrl Pts',(0.0379781508110965,-0.133926497290667,
1.39726217616581));
#15857=CARTESIAN_POINT('Ctrl Pts',(0.133119345865688,-0.0407171622080862,
1.40520116580311));
#15858=CARTESIAN_POINT('Ctrl Pts',(0.106398871137127,0.0897659150453452,
1.41314015544042));
#15859=CARTESIAN_POINT('Ctrl Pts',(-0.0177224175491345,0.138074504763813,
1.42107914507772));
#15860=CARTESIAN_POINT('Ctrl Pts',(-0.105714817800915,0.0743914165933911,
1.42755352277305));
#15861=CARTESIAN_POINT('Ctrl Pts',(-0.11763602712824,0.0175874039095825,
1.43138157058926));
#15862=CARTESIAN_POINT('Ctrl Pts',(-0.117590702341447,3.39534724351446E-5,
1.43256328852638));
#15863=CARTESIAN_POINT('Ctrl Pts',(-0.117613151267609,6.1407627239024E-5,
1.39243671147361));
#15864=CARTESIAN_POINT('Ctrl Pts',(-0.117501644803633,-0.0235525549213426,
1.39402718828666));
#15865=CARTESIAN_POINT('Ctrl Pts',(-0.0991469449676741,-0.0866320980727062,
1.39826505447396));
#15866=CARTESIAN_POINT('Ctrl Pts',(0.00373660876362508,-0.139175849115243,
1.40515031003553));
#15867=CARTESIAN_POINT('Ctrl Pts',(0.118990018389619,-0.0722858665142316,
1.41309247815831));
#15868=CARTESIAN_POINT('Ctrl Pts',(0.125236419206141,0.0608253567263532,
1.42103464628109));
#15869=CARTESIAN_POINT('Ctrl Pts',(0.0167532566496359,0.13821437898841,
1.42897681440387));
#15870=CARTESIAN_POINT('Ctrl Pts',(-0.0944771051913143,0.0939940009069027,
1.43611083613471));
#15871=CARTESIAN_POINT('Ctrl Pts',(-0.117474319425011,0.0271612872365273,
1.44059746849129));
#15872=CARTESIAN_POINT('Ctrl Pts',(-0.117692994131604,-9.9598288229346E-5,
1.44243671147361));
#15873=CARTESIAN_POINT('Origin',(0.,0.,-0.0924367114736175));
#15874=CARTESIAN_POINT('',(-0.117871679003533,-9.01049542302267E-5,1.33256328852638));
#15875=CARTESIAN_POINT('',(-0.117917347702326,6.89762296073142E-5,1.34243671147361));
#15876=CARTESIAN_POINT('',(-0.117775,2.85464118895969E-14,-0.0924367114736175));
#15877=CARTESIAN_POINT('Ctrl Pts',(-0.117871679003533,-9.01049542302501E-5,
1.33256328852638));
#15878=CARTESIAN_POINT('Ctrl Pts',(-0.117921183610054,-0.00593170075121234,
1.33295894537338));
#15879=CARTESIAN_POINT('Ctrl Pts',(-0.114870949065289,-0.0507926200311143,
1.33600093209947));
#15880=CARTESIAN_POINT('Ctrl Pts',(-0.0572704544775333,-0.126880813469472,
1.34168924870467));
#15881=CARTESIAN_POINT('Ctrl Pts',(0.0755477687720905,-0.116923823242002,
1.34962823834197));
#15882=CARTESIAN_POINT('Ctrl Pts',(0.13920718769651,6.89141801743488E-5,
1.35756722797928));
#15883=CARTESIAN_POINT('Ctrl Pts',(0.0754319660950179,0.116998564767658,
1.36550621761658));
#15884=CARTESIAN_POINT('Ctrl Pts',(-0.0573960494825499,0.126824048933643,
1.37344520725389));
#15885=CARTESIAN_POINT('Ctrl Pts',(-0.11489462347839,0.0507140179075799,
1.37913089755716));
#15886=CARTESIAN_POINT('Ctrl Pts',(-0.117921788132912,0.00589240827474643,
1.38217025798132));
#15887=CARTESIAN_POINT('Ctrl Pts',(-0.117872752581409,8.97255421561322E-5,
1.38256328852638));
#15888=CARTESIAN_POINT('Ctrl Pts',(-0.117917347702326,6.89762296073276E-5,
1.34243671147361));
#15889=CARTESIAN_POINT('Ctrl Pts',(-0.117673982084908,-0.0349283870656527,
1.34480951870776));
#15890=CARTESIAN_POINT('Ctrl Pts',(-0.0826049238592893,-0.109396528181867,
1.34982971531618));
#15891=CARTESIAN_POINT('Ctrl Pts',(0.0440301174146577,-0.132080378229483,
1.35749730129884));
#15892=CARTESIAN_POINT('Ctrl Pts',(0.13486394497766,-0.0345773583278084,
1.36543946942163));
#15893=CARTESIAN_POINT('Ctrl Pts',(0.102148545386143,0.0946020732301706,
1.3733816375444));
#15894=CARTESIAN_POINT('Ctrl Pts',(-0.0241454188302812,0.137116288461919,
1.38132380566719));
#15895=CARTESIAN_POINT('Ctrl Pts',(-0.107458038693719,0.07065895059964,
1.38767549697692));
#15896=CARTESIAN_POINT('Ctrl Pts',(-0.117687250167678,0.015753490298928,
1.3913797989124));
#15897=CARTESIAN_POINT('Ctrl Pts',(-0.117613151267609,6.1407627239024E-5,
1.39243671147361));
#15898=CARTESIAN_POINT('Origin',(0.,0.,-0.0924367114736175));
#15899=CARTESIAN_POINT('',(-0.117590388001671,-3.33269891443968E-5,1.28256328852638));
#15900=CARTESIAN_POINT('',(-0.117823716245033,-0.000102811805890834,1.29243671147362));
#15901=CARTESIAN_POINT('',(-0.117775,2.85464118895969E-14,-0.0924367114736175));
#15902=CARTESIAN_POINT('Ctrl Pts',(-0.117590388001671,-3.33269891444124E-5,
1.28256328852638));
#15903=CARTESIAN_POINT('Ctrl Pts',(-0.117634977734708,-0.017625925033684,
1.28374763276543));
#15904=CARTESIAN_POINT('Ctrl Pts',(-0.105676786131388,-0.0744702911817869,
1.28757830688358));
#15905=CARTESIAN_POINT('Ctrl Pts',(-0.0175857351491984,-0.138091953858251,
1.29405531088083));
#15906=CARTESIAN_POINT('Ctrl Pts',(0.106487712804436,-0.089660542174548,
1.30199430051814));
#15907=CARTESIAN_POINT('Ctrl Pts',(0.133078957772855,0.0408489510387311,
1.30993329015544));
#15908=CARTESIAN_POINT('Ctrl Pts',(0.0378455373822902,0.133964029124136,
1.31787227979275));
#15909=CARTESIAN_POINT('Ctrl Pts',(-0.0855601048685178,0.105915403748908,
1.32541561258306));
#15910=CARTESIAN_POINT('Ctrl Pts',(-0.117590074669608,0.0331395035428114,
1.33031261549427));
#15911=CARTESIAN_POINT('Ctrl Pts',(-0.117871679003533,-9.01049542302501E-5,
1.33256328852638));
#15912=CARTESIAN_POINT('Ctrl Pts',(-0.117823716245033,-0.000102811805890825,
1.29243671147362));
#15913=CARTESIAN_POINT('Ctrl Pts',(-0.117892441435953,-0.00760726064997237,
1.29294445975461));
#15914=CARTESIAN_POINT('Ctrl Pts',(-0.113819337750002,-0.0541654333254181,
1.29609959740987));
#15915=CARTESIAN_POINT('Ctrl Pts',(-0.0518146499729274,-0.129225073214149,
1.30190212443939));
#15916=CARTESIAN_POINT('Ctrl Pts',(0.0805213734929343,-0.11357898534207,
1.30984429256217));
#15917=CARTESIAN_POINT('Ctrl Pts',(0.1390915465469,0.0061171215252809,1.31778646068495));
#15918=CARTESIAN_POINT('Ctrl Pts',(0.0702395735793815,0.120209316621791,
1.32572862880773));
#15919=CARTESIAN_POINT('Ctrl Pts',(-0.0629590648350173,0.124177428154433,
1.33367079693051));
#15920=CARTESIAN_POINT('Ctrl Pts',(-0.115917830154768,0.0471875384414626,
1.33924015781913));
#15921=CARTESIAN_POINT('Ctrl Pts',(-0.117945510062545,0.00411888419242175,
1.3421621293335));
#15922=CARTESIAN_POINT('Ctrl Pts',(-0.117917347702326,6.89762296073276E-5,
1.34243671147361));
#15923=CARTESIAN_POINT('Origin',(0.,0.,-0.0924367114736175));
#15924=CARTESIAN_POINT('',(-0.11774949833287,0.000107383800510985,1.23256328852638));
#15925=CARTESIAN_POINT('',(-0.117581795058195,-8.20683476789735E-6,1.24243671147361));
#15926=CARTESIAN_POINT('',(-0.117775,2.85464118895969E-14,-0.0924367114736175));
#15927=CARTESIAN_POINT('Ctrl Pts',(-0.11774949833287,0.000107383800510997,
1.23256328852638));
#15928=CARTESIAN_POINT('Ctrl Pts',(-0.1174869159147,-0.0291008736543001,
1.23453632015749));
#15929=CARTESIAN_POINT('Ctrl Pts',(-0.0917482398636095,-0.0978979247776974,
1.23915568166769));
#15930=CARTESIAN_POINT('Ctrl Pts',(0.0236422145726536,-0.137184880695923,
1.246421373057));
#15931=CARTESIAN_POINT('Ctrl Pts',(0.128082862902196,-0.0545291301253663,
1.2543603626943));
#15932=CARTESIAN_POINT('Ctrl Pts',(0.115272428336817,0.0780443019497631,
1.26229935233161));
#15933=CARTESIAN_POINT('Ctrl Pts',(-0.00306201423577413,0.139173524314926,
1.27023834196891));
#15934=CARTESIAN_POINT('Ctrl Pts',(-0.101358337705897,0.08278581645186,
1.27699298736717));
#15935=CARTESIAN_POINT('Ctrl Pts',(-0.117535345263889,0.02168343817453,
1.28110130288633));
#15936=CARTESIAN_POINT('Ctrl Pts',(-0.117590388001671,-3.33269891444124E-5,
1.28256328852638));
#15937=CARTESIAN_POINT('Ctrl Pts',(-0.117581795058195,-8.20683476789562E-6,
1.24243671147361));
#15938=CARTESIAN_POINT('Ctrl Pts',(-0.117593699448189,-0.0191748937105988,
1.24372679017572));
#15939=CARTESIAN_POINT('Ctrl Pts',(-0.104100832827715,-0.0776580224685839,
1.24766425825208));
#15940=CARTESIAN_POINT('Ctrl Pts',(-0.0120149744006178,-0.138706589206355,
1.25424911570271));
#15941=CARTESIAN_POINT('Ctrl Pts',(0.110059129405696,-0.0852693704304675,
1.26219128382548));
#15942=CARTESIAN_POINT('Ctrl Pts',(0.13130776387206,0.0462833517151888,
1.27013345194827));
#15943=CARTESIAN_POINT('Ctrl Pts',(0.0322649968732001,0.135435768819968,
1.27807562007105));
#15944=CARTESIAN_POINT('Ctrl Pts',(-0.0881142830049797,0.102747609761224,
1.28551003991283));
#15945=CARTESIAN_POINT('Ctrl Pts',(-0.117534109666069,0.0315207854174475,
1.29029707038035));
#15946=CARTESIAN_POINT('Ctrl Pts',(-0.117823716245033,-0.000102811805890825,
1.29243671147362));
#15947=CARTESIAN_POINT('Origin',(0.,0.,-0.0924367114736175));
#15948=CARTESIAN_POINT('',(-0.117957988745754,-3.12301727557783E-5,1.18256328852638));
#15949=CARTESIAN_POINT('',(-0.117793553451004,0.000106755881474893,1.19243671147362));
#15950=CARTESIAN_POINT('',(-0.117775,2.85464118895969E-14,-0.0924367114736175));
#15951=CARTESIAN_POINT('Ctrl Pts',(-0.117957988745754,-3.12301727557569E-5,
1.18256328852638));
#15952=CARTESIAN_POINT('Ctrl Pts',(-0.117964007145535,-0.00173159226684161,
1.18267867767044));
#15953=CARTESIAN_POINT('Ctrl Pts',(-0.117160216762375,-0.0424221720604921,
1.1854403966936));
#15954=CARTESIAN_POINT('Ctrl Pts',(-0.0703321751825429,-0.12013338809653,
1.19084844559586));
#15955=CARTESIAN_POINT('Ctrl Pts',(0.0627954496153871,-0.124239193932754,
1.19878743523316));
#15956=CARTESIAN_POINT('Ctrl Pts',(0.138438143943654,-0.0146125323915816,
1.20672642487047));
#15957=CARTESIAN_POINT('Ctrl Pts',(0.0873502052771435,0.108390901091839,
1.21466541450777));
#15958=CARTESIAN_POINT('Ctrl Pts',(-0.043700859820065,0.132169893139269,
1.22260440414508));
#15959=CARTESIAN_POINT('Ctrl Pts',(-0.112119660921406,0.0591163174148552,
1.22857036215128));
#15960=CARTESIAN_POINT('Ctrl Pts',(-0.117839104743291,0.0100747194789664,
1.23188999027838));
#15961=CARTESIAN_POINT('Ctrl Pts',(-0.11774949833287,0.000107383800510997,
1.23256328852638));
#15962=CARTESIAN_POINT('Ctrl Pts',(-0.117793553451004,0.000106755881474891,
1.19243671147362));
#15963=CARTESIAN_POINT('Ctrl Pts',(-0.117510050331475,-0.0305433296418112,
1.19450912059683));
#15964=CARTESIAN_POINT('Ctrl Pts',(-0.0896091397727994,-0.100804620014092,
1.19922891909429));
#15965=CARTESIAN_POINT('Ctrl Pts',(0.0288222657999454,-0.136209964735594,
1.20659610696603));
#15966=CARTESIAN_POINT('Ctrl Pts',(0.130092623711363,-0.0495962373069701,
1.21453827508881));
#15967=CARTESIAN_POINT('Ctrl Pts',(0.112184773380136,0.082452738709893,
1.22248044321158));
#15968=CARTESIAN_POINT('Ctrl Pts',(-0.00849585454694533,0.138966535376798,
1.23042261133437));
#15969=CARTESIAN_POINT('Ctrl Pts',(-0.103054997843392,0.079672038485689,
1.23707470075504));
#15970=CARTESIAN_POINT('Ctrl Pts',(-0.11756927027536,0.0201573447738481,
1.24107940080146));
#15971=CARTESIAN_POINT('Ctrl Pts',(-0.117581795058195,-8.20683476789562E-6,
1.24243671147361));
#15972=CARTESIAN_POINT('Origin',(0.,0.,-0.0924367114736175));
#15973=CARTESIAN_POINT('',(-0.117657565919426,-8.78585414499747E-5,1.13256328852638));
#15974=CARTESIAN_POINT('',(-0.117937823388479,-5.4172489969917E-5,1.14243671147362));
#15975=CARTESIAN_POINT('',(-0.117775,2.85464118895969E-14,-0.0924367114736175));
#15976=CARTESIAN_POINT('Ctrl Pts',(-0.117657565919426,-8.78585414499974E-5,
1.13256328852638));
#15977=CARTESIAN_POINT('Ctrl Pts',(-0.11775046973706,-0.0134980674796043,
1.13346736506249));
#15978=CARTESIAN_POINT('Ctrl Pts',(-0.109441032251172,-0.0660497484721492,
1.13701777147771));
#15979=CARTESIAN_POINT('Ctrl Pts',(-0.0320511128216771,-0.13546723577438,
1.14321450777202));
#15980=CARTESIAN_POINT('Ctrl Pts',(0.0964380908528195,-0.100390938007982,
1.15115349740933));
#15981=CARTESIAN_POINT('Ctrl Pts',(0.136644831685568,0.0265863832644056,
1.15909248704664));
#15982=CARTESIAN_POINT('Ctrl Pts',(0.0517625939920979,0.129225692742072,
1.16703147668394));
#15983=CARTESIAN_POINT('Ctrl Pts',(-0.0785823129332351,0.113795317289389,
1.17485507717719));
#15984=CARTESIAN_POINT('Ctrl Pts',(-0.117825981412732,0.0372644419932696,
1.18003234779134));
#15985=CARTESIAN_POINT('Ctrl Pts',(-0.117957988745754,-3.12301727557569E-5,
1.18256328852638));
#15986=CARTESIAN_POINT('Ctrl Pts',(-0.117937823388479,-5.41724899699178E-5,
1.14243671147362));
#15987=CARTESIAN_POINT('Ctrl Pts',(-0.117955293269658,-0.0031110520517566,
1.14264406164367));
#15988=CARTESIAN_POINT('Ctrl Pts',(-0.116460933142332,-0.0451799670343263,
1.14549880118799));
#15989=CARTESIAN_POINT('Ctrl Pts',(-0.0660858892268601,-0.122541963197144,
1.15100093010657));
#15990=CARTESIAN_POINT('Ctrl Pts',(0.0671705316110708,-0.121950798202395,
1.15894309822935));
#15991=CARTESIAN_POINT('Ctrl Pts',(0.138891844802359,-0.00964017357273747,
1.16688526635212));
#15992=CARTESIAN_POINT('Ctrl Pts',(0.0833739592533277,0.111501840422208,
1.17482743447491));
#15993=CARTESIAN_POINT('Ctrl Pts',(-0.0485230383040216,0.130496713571114,
1.18276960259768));
#15994=CARTESIAN_POINT('Ctrl Pts',(-0.113150295826959,0.0561813708375219,
1.18863936159726));
#15995=CARTESIAN_POINT('Ctrl Pts',(-0.117872210070015,0.00861047923971886,
1.19186173122257));
#15996=CARTESIAN_POINT('Ctrl Pts',(-0.117793553451004,0.000106755881474891,
1.19243671147362));
#15997=CARTESIAN_POINT('Origin',(0.,0.,-0.0924367114736175));
#15998=CARTESIAN_POINT('',(-0.117641451221435,8.0229283111194E-5,1.08256328852638));
#15999=CARTESIAN_POINT('',(-0.117630591849015,-7.42484764288953E-5,1.09243671147362));
#16000=CARTESIAN_POINT('',(-0.117775,2.85464118895969E-14,-0.0924367114736175));
#16001=CARTESIAN_POINT('Ctrl Pts',(-0.117641451221435,8.02292831111745E-5,
1.08256328852638));
#16002=CARTESIAN_POINT('Ctrl Pts',(-0.117483998834985,-0.0250372639622414,
1.08425605245455));
#16003=CARTESIAN_POINT('Ctrl Pts',(-0.0972946570053161,-0.0896524615425008,
1.08859514626182));
#16004=CARTESIAN_POINT('Ctrl Pts',(0.00904258428980543,-0.13891320121148,
1.09558056994819));
#16005=CARTESIAN_POINT('Ctrl Pts',(0.121617839487272,-0.067732908692211,
1.1035195595855));
#16006=CARTESIAN_POINT('Ctrl Pts',(0.122860297649024,0.0654522196953821,
1.1114585492228));
#16007=CARTESIAN_POINT('Ctrl Pts',(0.0116325734791967,0.138720326685422,
1.11939753886011));
#16008=CARTESIAN_POINT('Ctrl Pts',(-0.096364912740844,0.0911171059582243,
1.1264324519613));
#16009=CARTESIAN_POINT('Ctrl Pts',(-0.117478530206868,0.0257550656131636,
1.13082103518339));
#16010=CARTESIAN_POINT('Ctrl Pts',(-0.117657565919426,-8.78585414499974E-5,
1.13256328852638));
#16011=CARTESIAN_POINT('Ctrl Pts',(-0.117630591849015,-7.42484764288814E-5,
1.09243671147362));
#16012=CARTESIAN_POINT('Ctrl Pts',(-0.117715241483118,-0.0147626739157663,
1.09342639206478));
#16013=CARTESIAN_POINT('Ctrl Pts',(-0.108350501834675,-0.0686384992808382,
1.0970634620302));
#16014=CARTESIAN_POINT('Ctrl Pts',(-0.0276126195379174,-0.136460326620484,
1.10334792136989));
#16015=CARTESIAN_POINT('Ctrl Pts',(0.0997182217817603,-0.0971604536002107,
1.11129008949267));
#16016=CARTESIAN_POINT('Ctrl Pts',(0.135696927507188,0.0311483765905046,
1.11923225761545));
#16017=CARTESIAN_POINT('Ctrl Pts',(0.0473633069609982,0.130922093830007,
1.12717442573822));
#16018=CARTESIAN_POINT('Ctrl Pts',(-0.0809210029008042,0.111284164335459,
1.13490924369095));
#16019=CARTESIAN_POINT('Ctrl Pts',(-0.117732242679493,0.0359183370635313,
1.13999667226941));
#16020=CARTESIAN_POINT('Ctrl Pts',(-0.117937823388479,-5.41724899699178E-5,
1.14243671147362));
#16021=CARTESIAN_POINT('Origin',(0.,0.,-0.0924367114736175));
#16022=CARTESIAN_POINT('',(-0.117948158721073,4.38502512853227E-5,1.03256328852638));
#16023=CARTESIAN_POINT('',(-0.117667547954054,9.20194976846214E-5,1.04243671147362));
#16024=CARTESIAN_POINT('',(-0.117775,2.85464118895969E-14,-0.0924367114736175));
#16025=CARTESIAN_POINT('Ctrl Pts',(-0.117948158721073,4.38502512853157E-5,
1.03256328852638));
#16026=CARTESIAN_POINT('Ctrl Pts',(-0.117773439871091,-0.0365306738650768,
1.03504473984661));
#16027=CARTESIAN_POINT('Ctrl Pts',(-0.0798690478914953,-0.112422454385097,
1.04017252104593));
#16028=CARTESIAN_POINT('Ctrl Pts',(0.0493427524230464,-0.130168884856471,
1.04794663212436));
#16029=CARTESIAN_POINT('Ctrl Pts',(0.136125055048066,-0.0291310004912345,
1.05588562176166));
#16030=CARTESIAN_POINT('Ctrl Pts',(0.0982941990358779,0.0985743183458784,
1.06382461139897));
#16031=CARTESIAN_POINT('Ctrl Pts',(-0.0295182596522469,0.136041604476578,
1.07176360103627));
#16032=CARTESIAN_POINT('Ctrl Pts',(-0.108818061611988,0.067537217334308,
1.07800982674541));
#16033=CARTESIAN_POINT('Ctrl Pts',(-0.11773014713001,0.0142293884972668,
1.08160972257545));
#16034=CARTESIAN_POINT('Ctrl Pts',(-0.117641451221435,8.02292831111745E-5,
1.08256328852638));
#16035=CARTESIAN_POINT('Ctrl Pts',(-0.117667547954054,9.20194976846197E-5,
1.04243671147362));
#16036=CARTESIAN_POINT('Ctrl Pts',(-0.117475882803567,-0.0261866690710452,
1.04420872248589));
#16037=CARTESIAN_POINT('Ctrl Pts',(-0.0957916308421219,-0.0920126959480487,
1.04862812287242));
#16038=CARTESIAN_POINT('Ctrl Pts',(0.0132451643780021,-0.13859452774087,
1.05569491263321));
#16039=CARTESIAN_POINT('Ctrl Pts',(0.123654649330263,-0.0639797248987874,
1.06363708075599));
#16040=CARTESIAN_POINT('Ctrl Pts',(0.120783771971213,0.0692470788374567,
1.07157924887876));
#16041=CARTESIAN_POINT('Ctrl Pts',(0.00726255089817806,0.139036444335888,
1.07952141700155));
#16042=CARTESIAN_POINT('Ctrl Pts',(-0.0979368667310299,0.0886295245336828,
1.08647390453316));
#16043=CARTESIAN_POINT('Ctrl Pts',(-0.117488804242801,0.0245287720112504,
1.09077900269052));
#16044=CARTESIAN_POINT('Ctrl Pts',(-0.117630591849015,-7.42484764288814E-5,
1.09243671147362));
#16045=CARTESIAN_POINT('Origin',(0.,0.,-0.0924367114736175));
#16046=CARTESIAN_POINT('',(-0.117771476475648,-0.000107683352847938,0.982563288526384));
#16047=CARTESIAN_POINT('',(-0.11796176292438,2.53781033017321E-5,0.992436711473616));
#16048=CARTESIAN_POINT('',(-0.117775,2.85464118895969E-14,-0.0924367114736175));
#16049=CARTESIAN_POINT('Ctrl Pts',(-0.117771476475648,-0.000107683352847945,
0.982563288526384));
#16050=CARTESIAN_POINT('Ctrl Pts',(-0.117856103358663,-0.00933799346614349,
0.983187097359559));
#16051=CARTESIAN_POINT('Ctrl Pts',(-0.112646870919438,-0.057630810124202,
0.986457236071836));
#16052=CARTESIAN_POINT('Ctrl Pts',(-0.0461590140787468,-0.131331607851033,
0.992373704663214));
#16053=CARTESIAN_POINT('Ctrl Pts',(0.0853128637208732,-0.110001641284132,
1.00031269430052));
#16054=CARTESIAN_POINT('Ctrl Pts',(0.138686661656432,0.0120272889735618,
1.00825168393783));
#16055=CARTESIAN_POINT('Ctrl Pts',(0.0651023256631918,0.123046060459907,
1.01619067357513));
#16056=CARTESIAN_POINT('Ctrl Pts',(-0.0680787277209358,0.121424596492465,
1.02412966321244));
#16057=CARTESIAN_POINT('Ctrl Pts',(-0.116790117880403,0.0438975063746073,
1.02958720152952));
#16058=CARTESIAN_POINT('Ctrl Pts',(-0.11795976781127,0.00247402277930658,
1.0323984099675));
#16059=CARTESIAN_POINT('Ctrl Pts',(-0.117948158721073,4.38502512853157E-5,
1.03256328852638));
#16060=CARTESIAN_POINT('Ctrl Pts',(-0.11796176292438,2.53781033017319E-5,
0.992436711473616));
#16061=CARTESIAN_POINT('Ctrl Pts',(-0.117851518882229,-0.0376119105440478,
0.994991052906992));
#16062=CARTESIAN_POINT('Ctrl Pts',(-0.077958511321084,-0.114458475672252,
1.00019278371463));
#16063=CARTESIAN_POINT('Ctrl Pts',(0.0529591494285269,-0.128760265574912,
1.00804190389653));
#16064=CARTESIAN_POINT('Ctrl Pts',(0.136912761112491,-0.0252739657289669,
1.0159840720193));
#16065=CARTESIAN_POINT('Ctrl Pts',(0.0954402180350474,0.101365883217864,
1.02392624014209));
#16066=CARTESIAN_POINT('Ctrl Pts',(-0.0334653697086341,0.135144169424284,
1.03186840826486));
#16067=CARTESIAN_POINT('Ctrl Pts',(-0.109792739119276,0.0652029671457737,
1.03803856537538));
#16068=CARTESIAN_POINT('Ctrl Pts',(-0.117762231070763,0.0130737646421874,
1.04156133311163));
#16069=CARTESIAN_POINT('Ctrl Pts',(-0.117667547954054,9.20194976846197E-5,
1.04243671147362));
#16070=CARTESIAN_POINT('Origin',(0.,0.,-0.0924367114736175));
#16071=CARTESIAN_POINT('',(-0.117585265278523,2.16484251076657E-5,0.932563288526384));
#16072=CARTESIAN_POINT('',(-0.117742563953077,-0.000107211314308964,0.942436711473616));
#16073=CARTESIAN_POINT('',(-0.117775,2.85464118895969E-14,-0.0924367114736175));
#16074=CARTESIAN_POINT('Ctrl Pts',(-0.117585265278523,2.16484251076635E-5,
0.932563288526384));
#16075=CARTESIAN_POINT('Ctrl Pts',(-0.117550805757046,-0.0209622679161363,
0.933975784751614));
#16076=CARTESIAN_POINT('Ctrl Pts',(-0.102172791552808,-0.0813069697478888,
0.938034610855947));
#16077=CARTESIAN_POINT('Ctrl Pts',(-0.00565790085648466,-0.139092177922979,
0.944739766839381));
#16078=CARTESIAN_POINT('Ctrl Pts',(0.113796373024222,-0.0801812402497705,
0.952678756476687));
#16079=CARTESIAN_POINT('Ctrl Pts',(0.129077866376032,0.0521301276928276,
0.960617746113992));
#16080=CARTESIAN_POINT('Ctrl Pts',(0.026197419344502,0.13671993644362,0.968556735751298));
#16081=CARTESIAN_POINT('Ctrl Pts',(-0.0906967139502387,0.0993396518733501,
0.975871916555428));
#16082=CARTESIAN_POINT('Ctrl Pts',(-0.117497098103867,0.02981894716558,
0.980540767480457));
#16083=CARTESIAN_POINT('Ctrl Pts',(-0.117771476475648,-0.000107683352847945,
0.982563288526384));
#16084=CARTESIAN_POINT('Ctrl Pts',(-0.117742563953077,-0.000107211314308957,
0.942436711473616));
#16085=CARTESIAN_POINT('Ctrl Pts',(-0.117833632602859,-0.0103126986533654,
0.943125993953839));
#16086=CARTESIAN_POINT('Ctrl Pts',(-0.111944766202914,-0.0596118697348184,
0.946462665808322));
#16087=CARTESIAN_POINT('Ctrl Pts',(-0.0428565117498991,-0.132465832952297,
0.952446727037066));
#16088=CARTESIAN_POINT('Ctrl Pts',(0.0880997963686447,-0.107806787258123,
0.960388895159846));
#16089=CARTESIAN_POINT('Ctrl Pts',(0.138347640177547,0.0156143509765511,
0.968331063282625));
#16090=CARTESIAN_POINT('Ctrl Pts',(0.061854832590724,0.124731139593481,
0.976273231405407));
#16091=CARTESIAN_POINT('Ctrl Pts',(-0.0713033562375951,0.119581390225944,
0.984215399528185));
#16092=CARTESIAN_POINT('Ctrl Pts',(-0.117322772537986,0.0417718924351975,
0.989603226217589));
#16093=CARTESIAN_POINT('Ctrl Pts',(-0.11796577882491,0.00139640554830399,
0.992343663532733));
#16094=CARTESIAN_POINT('Ctrl Pts',(-0.11796176292438,2.53781033017319E-5,
0.992436711473616));
#16095=CARTESIAN_POINT('Origin',(0.,0.,-0.0924367114736175));
#16096=CARTESIAN_POINT('',(-0.117850913371472,9.6525574830472E-5,0.882563288526384));
#16097=CARTESIAN_POINT('',(-0.117591231449503,3.54948526558943E-5,0.892436711473616));
#16098=CARTESIAN_POINT('',(-0.117775,2.85464118895969E-14,-0.0924367114736175));
#16099=CARTESIAN_POINT('Ctrl Pts',(-0.117850913371472,9.65255748304767E-5,
0.882563288526384));
#16100=CARTESIAN_POINT('Ctrl Pts',(-0.117563006813672,-0.0324172738354332,
0.884764472143669));
#16101=CARTESIAN_POINT('Ctrl Pts',(-0.0867151192651892,-0.104499852648429,
0.889611985640057));
#16102=CARTESIAN_POINT('Ctrl Pts',(0.0353397195745277,-0.134646760160997,
0.897105829015547));
#16103=CARTESIAN_POINT('Ctrl Pts',(0.132293719443212,-0.0433245611326863,
0.905044818652852));
#16104=CARTESIAN_POINT('Ctrl Pts',(0.108141885842356,0.0876583043865096,
0.912983808290157));
#16105=CARTESIAN_POINT('Ctrl Pts',(-0.0150064327997127,0.138395999855801,
0.920922797927463));
#16106=CARTESIAN_POINT('Ctrl Pts',(-0.104951114476159,0.0759553573435841,
0.927449291339539));
#16107=CARTESIAN_POINT('Ctrl Pts',(-0.117615366114572,0.01835136974357,
0.931329454872513));
#16108=CARTESIAN_POINT('Ctrl Pts',(-0.117585265278523,2.16484251076635E-5,
0.932563288526384));
#16109=CARTESIAN_POINT('Ctrl Pts',(-0.117591231449503,3.54948526559117E-5,
0.892436711473616));
#16110=CARTESIAN_POINT('Ctrl Pts',(-0.117532234588281,-0.0218238662162972,
0.893908324374946));
#16111=CARTESIAN_POINT('Ctrl Pts',(-0.101194437785642,-0.0830895288483654,
0.898027326650536));
#16112=CARTESIAN_POINT('Ctrl Pts',(-0.00250162451743248,-0.139203517821528,
0.904793718300386));
#16113=CARTESIAN_POINT('Ctrl Pts',(0.115632500949424,-0.0775435504945224,
0.912735886423165));
#16114=CARTESIAN_POINT('Ctrl Pts',(0.127835376168433,0.0551542754370876,
0.920678054545947));
#16115=CARTESIAN_POINT('Ctrl Pts',(0.0229279137899797,0.137325118854324,
0.928620222668725));
#16116=CARTESIAN_POINT('Ctrl Pts',(-0.0920562790907298,0.0974788594069619,
0.935873108311283));
#16117=CARTESIAN_POINT('Ctrl Pts',(-0.117483857027998,0.0288844367965532,
0.94047860457958));
#16118=CARTESIAN_POINT('Ctrl Pts',(-0.117742563953077,-0.000107211314308957,
0.942436711473616));
#16119=CARTESIAN_POINT('Origin',(0.,0.,-0.0924367114736175));
#16120=CARTESIAN_POINT('',(-0.11789232318732,-8.18790992476613E-5,0.832563288526384));
#16121=CARTESIAN_POINT('',(-0.117872825429845,8.99519344067963E-5,0.842436711473616));
#16122=CARTESIAN_POINT('',(-0.117775,2.85464118895969E-14,-0.0924367114736175));
#16123=CARTESIAN_POINT('Ctrl Pts',(-0.11789232318732,-8.18790992476734E-5,
0.832563288526384));
#16124=CARTESIAN_POINT('Ctrl Pts',(-0.117932494517479,-0.00515170743829337,
0.832906829656623));
#16125=CARTESIAN_POINT('Ctrl Pts',(-0.115332713682068,-0.0492334187378749,
0.835896700665964));
#16126=CARTESIAN_POINT('Ctrl Pts',(-0.059752088941783,-0.125731196083361,
0.841532901554406));
#16127=CARTESIAN_POINT('Ctrl Pts',(0.0732361146625898,-0.118385460722959,
0.849471891191712));
#16128=CARTESIAN_POINT('Ctrl Pts',(0.139181674492094,-0.00266594955618734,
0.857410880829018));
#16129=CARTESIAN_POINT('Ctrl Pts',(0.077715950067195,0.115494055719818,
0.865349870466323));
#16130=CARTESIAN_POINT('Ctrl Pts',(-0.0548934004223171,0.127927168308903,
0.87328886010363));
#16131=CARTESIAN_POINT('Ctrl Pts',(-0.114416768398411,0.0522742940766184,
0.879026666123649));
#16132=CARTESIAN_POINT('Ctrl Pts',(-0.117909136832228,0.0066718045071592,
0.882118142264567));
#16133=CARTESIAN_POINT('Ctrl Pts',(-0.117850913371472,9.65255748304767E-5,
0.882563288526384));
#16134=CARTESIAN_POINT('Ctrl Pts',(-0.117872825429845,8.99519344067998E-5,
0.842436711473616));
#16135=CARTESIAN_POINT('Ctrl Pts',(-0.117591169542271,-0.0331870933343037,
0.844690654796053));
#16136=CARTESIAN_POINT('Ctrl Pts',(-0.0854771005934613,-0.106025606004136,
0.84959198749275));
#16137=CARTESIAN_POINT('Ctrl Pts',(0.0380692928980519,-0.133920149482284,
0.857140709563706));
#16138=CARTESIAN_POINT('Ctrl Pts',(0.133179650076608,-0.0405839661022353,
0.865082877686486));
#16139=CARTESIAN_POINT('Ctrl Pts',(0.106283765719693,0.0899312995767124,
0.873025045809266));
#16140=CARTESIAN_POINT('Ctrl Pts',(-0.0179789669825735,0.138060255849953,
0.880967213932046));
#16141=CARTESIAN_POINT('Ctrl Pts',(-0.105798194743126,0.0742290978659706,
0.887437769153496));
#16142=CARTESIAN_POINT('Ctrl Pts',(-0.117638368248411,0.0175004969839459,
0.891260935000686));
#16143=CARTESIAN_POINT('Ctrl Pts',(-0.117591231449503,3.54948526559117E-5,
0.892436711473616));
#16144=CARTESIAN_POINT('Origin',(0.,0.,-0.0924367114736175));
#16145=CARTESIAN_POINT('',(-0.117598114366551,-4.51832715892789E-5,0.782563288526384));
#16146=CARTESIAN_POINT('',(-0.117874685330111,-8.92836445515327E-5,0.792436711473617));
#16147=CARTESIAN_POINT('',(-0.117775,2.85464118895969E-14,-0.0924367114736175));
#16148=CARTESIAN_POINT('Ctrl Pts',(-0.117598114366551,-4.518327158929E-5,
0.782563288526384));
#16149=CARTESIAN_POINT('Ctrl Pts',(-0.117656123976761,-0.0168608793038394,
0.783695517048678));
#16150=CARTESIAN_POINT('Ctrl Pts',(-0.106420815930739,-0.0729055463807818,
0.787474075450074));
#16151=CARTESIAN_POINT('Ctrl Pts',(-0.0202952816069424,-0.137719814645367,
0.793898963730571));
#16152=CARTESIAN_POINT('Ctrl Pts',(0.104705698854998,-0.0917352845351548,
0.801837953367879));
#16153=CARTESIAN_POINT('Ctrl Pts',(0.133855787965376,0.0382266115373486,
0.809776943005182));
#16154=CARTESIAN_POINT('Ctrl Pts',(0.0404700769297216,0.133194664588195,
0.81771593264249));
#16155=CARTESIAN_POINT('Ctrl Pts',(-0.0843190215395119,0.107398870964955,
0.825311381149555));
#16156=CARTESIAN_POINT('Ctrl Pts',(-0.117623050954756,0.0339016606582783,
0.830260499777521));
#16157=CARTESIAN_POINT('Ctrl Pts',(-0.11789232318732,-8.18790992476734E-5,
0.832563288526384));
#16158=CARTESIAN_POINT('Ctrl Pts',(-0.117874685330111,-8.9283644551537E-5,
0.792436711473617));
#16159=CARTESIAN_POINT('Ctrl Pts',(-0.11792303416021,-0.00583050672374999,
0.7928255958429));
#16160=CARTESIAN_POINT('Ctrl Pts',(-0.114931453360353,-0.0506053896743902,
0.795861869586443));
#16161=CARTESIAN_POINT('Ctrl Pts',(-0.0575513573065257,-0.126774282767806,
0.801545532704245));
#16162=CARTESIAN_POINT('Ctrl Pts',(0.0753527000357912,-0.117071978271622,
0.809487700827026));
#16163=CARTESIAN_POINT('Ctrl Pts',(0.139225942868322,-0.000119714417332432,
0.817429868949805));
#16164=CARTESIAN_POINT('Ctrl Pts',(0.0755539188089132,0.116942220141962,
0.825372037072586));
#16165=CARTESIAN_POINT('Ctrl Pts',(-0.0573332568284509,0.12687306712048,
0.833314205195366));
#16166=CARTESIAN_POINT('Ctrl Pts',(-0.114890414736801,0.0507419104293215,
0.839002429995709));
#16167=CARTESIAN_POINT('Ctrl Pts',(-0.117921990994851,0.00589875908008548,
0.842043265421793));
#16168=CARTESIAN_POINT('Ctrl Pts',(-0.117872825429845,8.99519344067998E-5,
0.842436711473616));
#16169=CARTESIAN_POINT('Origin',(0.,0.,-0.0924367114736175));
#16170=CARTESIAN_POINT('',(-0.11772691567491,0.000105512987197037,0.732563288526384));
#16171=CARTESIAN_POINT('',(-0.117591850253004,-3.65476421498312E-5,0.742436711473616));
#16172=CARTESIAN_POINT('',(-0.117775,2.85464118895969E-14,-0.0924367114736175));
#16173=CARTESIAN_POINT('Ctrl Pts',(-0.11772691567491,0.000105512987197042,
0.732563288526384));
#16174=CARTESIAN_POINT('Ctrl Pts',(-0.117479624464894,-0.0283451130369189,
0.734484204440733));
#16175=CARTESIAN_POINT('Ctrl Pts',(-0.0928318426870313,-0.096374559506161,
0.739051450234184));
#16176=CARTESIAN_POINT('Ctrl Pts',(0.0209425314183671,-0.137622876656644,
0.746265025906738));
#16177=CARTESIAN_POINT('Ctrl Pts',(0.126986869252672,-0.0570349089493802,
0.754204015544043));
#16178=CARTESIAN_POINT('Ctrl Pts',(0.11678343126468,0.0757646090434518,
0.762143005181349));
#16179=CARTESIAN_POINT('Ctrl Pts',(-0.000327234354877375,0.139206819944772,
0.770081994818654));
#16180=CARTESIAN_POINT('Ctrl Pts',(-0.100479183608201,0.0843410365921374,
0.776888755933667));
#16181=CARTESIAN_POINT('Ctrl Pts',(-0.117520539541507,0.0224420334666934,
0.781049187169576));
#16182=CARTESIAN_POINT('Ctrl Pts',(-0.117598114366551,-4.518327158929E-5,
0.782563288526384));
#16183=CARTESIAN_POINT('Ctrl Pts',(-0.117591850253004,-3.65476421498364E-5,
0.742436711473616));
#16184=CARTESIAN_POINT('Ctrl Pts',(-0.117640211257931,-0.0174335619022046,
0.743607926264006));
#16185=CARTESIAN_POINT('Ctrl Pts',(-0.105863856762799,-0.0740921523660566,
0.747426530428656));
#16186=CARTESIAN_POINT('Ctrl Pts',(-0.0182163644075178,-0.138029133036789,
0.753892523967566));
#16187=CARTESIAN_POINT('Ctrl Pts',(0.106128952536144,-0.0901139441634624,
0.761834692090347));
#16188=CARTESIAN_POINT('Ctrl Pts',(0.133249245915149,0.0403548753208232,
0.769776860213125));
#16189=CARTESIAN_POINT('Ctrl Pts',(0.0382995408207276,0.133854483197375,
0.777719028335907));
#16190=CARTESIAN_POINT('Ctrl Pts',(-0.0853693283863186,0.106155717082476,
0.785272312089402));
#16191=CARTESIAN_POINT('Ctrl Pts',(-0.117593892160246,0.0332537408718532,
0.79017820646864));
#16192=CARTESIAN_POINT('Ctrl Pts',(-0.117874685330111,-8.9283644551537E-5,
0.792436711473617));
#16193=CARTESIAN_POINT('Origin',(0.,0.,-0.0924367114736175));
#16194=CARTESIAN_POINT('',(-0.117964947617991,-1.73329198795185E-5,0.682563288526384));
#16195=CARTESIAN_POINT('',(-0.117740574064672,0.000107068518266168,0.692436711473616));
#16196=CARTESIAN_POINT('',(-0.117775,2.85464118895969E-14,-0.0924367114736175));
#16197=CARTESIAN_POINT('Ctrl Pts',(-0.117964947617991,-1.73329198795367E-5,
0.682563288526384));
#16198=CARTESIAN_POINT('Ctrl Pts',(-0.117966864156947,-0.000949576032666658,
0.682626561953687));
#16199=CARTESIAN_POINT('Ctrl Pts',(-0.117534558560489,-0.0408698671952461,
0.685336165260092));
#16200=CARTESIAN_POINT('Ctrl Pts',(-0.0726787294560835,-0.118728463672822,
0.690692098445597));
#16201=CARTESIAN_POINT('Ctrl Pts',(0.0603425395611779,-0.125448888878168,
0.698631088082904));
#16202=CARTESIAN_POINT('Ctrl Pts',(0.138124349154501,-0.0173294538893964,
0.706570077720209));
#16203=CARTESIAN_POINT('Ctrl Pts',(0.0894627833767505,0.106653908470079,
0.714509067357515));
#16204=CARTESIAN_POINT('Ctrl Pts',(-0.0410958292974484,0.133002927094911,
0.72244805699482));
#16205=CARTESIAN_POINT('Ctrl Pts',(-0.111546724107196,0.0606813038481789,
0.728466130717777));
#16206=CARTESIAN_POINT('Ctrl Pts',(-0.117820302634623,0.0108495967181263,
0.731837874561632));
#16207=CARTESIAN_POINT('Ctrl Pts',(-0.11772691567491,0.000105512987197042,
0.732563288526384));
#16208=CARTESIAN_POINT('Ctrl Pts',(-0.117740574064672,0.000107068518266165,
0.692436711473616));
#16209=CARTESIAN_POINT('Ctrl Pts',(-0.117483171888848,-0.0288182833237499,
0.694390256685113));
#16210=CARTESIAN_POINT('Ctrl Pts',(-0.0921515028359353,-0.0973455904149804,
0.698991191270869));
#16211=CARTESIAN_POINT('Ctrl Pts',(0.022691720100341,-0.137364345221032,
0.706239515230886));
#16212=CARTESIAN_POINT('Ctrl Pts',(0.127740337615313,-0.0553740340325759,
0.714181683353665));
#16213=CARTESIAN_POINT('Ctrl Pts',(0.115765682611161,0.077344581120379,
0.722123851476446));
#16214=CARTESIAN_POINT('Ctrl Pts',(-0.00226223072526165,0.139207614056346,
0.730066019599226));
#16215=CARTESIAN_POINT('Ctrl Pts',(-0.101117998472899,0.083225715609228,
0.736836972931616));
#16216=CARTESIAN_POINT('Ctrl Pts',(-0.117530897055598,0.0218902846491045,
0.740960536889746));
#16217=CARTESIAN_POINT('Ctrl Pts',(-0.117591850253004,-3.65476421498364E-5,
0.742436711473616));
#16218=CARTESIAN_POINT('Origin',(0.,0.,-0.0924367114736175));
#16219=CARTESIAN_POINT('',(-0.117676160015555,-9.46906955630148E-5,0.632563288526383));
#16220=CARTESIAN_POINT('',(-0.117962383120995,-2.41598447144192E-5,0.642436711473616));
#16221=CARTESIAN_POINT('',(-0.117775,2.85464118895969E-14,-0.0924367114736175));
#16222=CARTESIAN_POINT('Ctrl Pts',(-0.117676160015555,-9.46906955630045E-5,
0.632563288526383));
#16223=CARTESIAN_POINT('Ctrl Pts',(-0.117771520970562,-0.0127268345011372,
0.633415249345741));
#16224=CARTESIAN_POINT('Ctrl Pts',(-0.110078248258936,-0.064483421762156,
0.636913540044201));
#16225=CARTESIAN_POINT('Ctrl Pts',(-0.0347063025259737,-0.134811417789573,
0.643058160621763));
#16226=CARTESIAN_POINT('Ctrl Pts',(0.0944472082050275,-0.102266175560326,
0.65099715025907));
#16227=CARTESIAN_POINT('Ctrl Pts',(0.137140772714236,0.0238967416356601,
0.658936139896373));
#16228=CARTESIAN_POINT('Ctrl Pts',(0.054291358674537,0.128183829614862,
0.666875129533682));
#16229=CARTESIAN_POINT('Ctrl Pts',(-0.0772016597727435,0.11523146575827,
0.674750845743682));
#16230=CARTESIAN_POINT('Ctrl Pts',(-0.117886707375211,0.0380402955314478,
0.679980232074585));
#16231=CARTESIAN_POINT('Ctrl Pts',(-0.117964947617991,-1.73329198795367E-5,
0.682563288526384));
#16232=CARTESIAN_POINT('Ctrl Pts',(-0.117962383120995,-2.41598447144253E-5,
0.642436711473616));
#16233=CARTESIAN_POINT('Ctrl Pts',(-0.117966033213387,-0.0013279541977536,
0.642525197731959));
#16234=CARTESIAN_POINT('Ctrl Pts',(-0.117355585052125,-0.0416360146359673,
0.645261073364563));
#16235=CARTESIAN_POINT('Ctrl Pts',(-0.0715088964667609,-0.119458592094588,
0.650644338371427));
#16236=CARTESIAN_POINT('Ctrl Pts',(0.0616402393688536,-0.124837327709565,
0.658586506494205));
#16237=CARTESIAN_POINT('Ctrl Pts',(0.138320583400205,-0.0158522461166236,
0.666528674616987));
#16238=CARTESIAN_POINT('Ctrl Pts',(0.0882850628235238,0.107655121482266,
0.674470842739765));
#16239=CARTESIAN_POINT('Ctrl Pts',(-0.0426286451686149,0.132539337972556,
0.682413010862546));
#16240=CARTESIAN_POINT('Ctrl Pts',(-0.111894847147975,0.059748848130285,
0.68840163377383));
#16241=CARTESIAN_POINT('Ctrl Pts',(-0.117831996057943,0.0103805377030848,
0.691742867310853));
#16242=CARTESIAN_POINT('Ctrl Pts',(-0.117740574064672,0.000107068518266165,
0.692436711473616));
#16243=CARTESIAN_POINT('Origin',(0.,0.,-0.0924367114736175));
#16244=CARTESIAN_POINT('',(-0.117626285855324,7.11112359239178E-5,0.582563288526384));
#16245=CARTESIAN_POINT('',(-0.11766919235599,-9.26074537421634E-5,0.592436711473616));
#16246=CARTESIAN_POINT('',(-0.117775,2.85464118895969E-14,-0.0924367114736175));
#16247=CARTESIAN_POINT('Ctrl Pts',(-0.117626285855324,7.11112359239024E-5,
0.582563288526383));
#16248=CARTESIAN_POINT('Ctrl Pts',(-0.117492102008102,-0.0242809575267813,
0.584203936737797));
#16249=CARTESIAN_POINT('Ctrl Pts',(-0.0982512120079041,-0.0881067492982899,
0.588490914828312));
#16250=CARTESIAN_POINT('Ctrl Pts',(0.00631176444456456,-0.139064040754811,
0.595424222797929));
#16251=CARTESIAN_POINT('Ctrl Pts',(0.120263693490807,-0.0701091280034811,
0.603363212435234));
#16252=CARTESIAN_POINT('Ctrl Pts',(0.124122453355413,0.0630258865426945,
0.611302202072541));
#16253=CARTESIAN_POINT('Ctrl Pts',(0.0143556138404206,0.138465021405133,
0.619241191709845));
#16254=CARTESIAN_POINT('Ctrl Pts',(-0.0953630726970595,0.0926558297308384,
0.626328220527794));
#16255=CARTESIAN_POINT('Ctrl Pts',(-0.117475314221613,0.0265106736450616,
0.630768919466639));
#16256=CARTESIAN_POINT('Ctrl Pts',(-0.117676160015555,-9.46906955630045E-5,
0.632563288526383));
#16257=CARTESIAN_POINT('Ctrl Pts',(-0.11766919235599,-9.26074537421669E-5,
0.592436711473616));
#16258=CARTESIAN_POINT('Ctrl Pts',(-0.117764072896019,-0.0130062487266101,
0.593307528153066));
#16259=CARTESIAN_POINT('Ctrl Pts',(-0.109848366281979,-0.0650658641993071,
0.596825734206776));
#16260=CARTESIAN_POINT('Ctrl Pts',(-0.0336977294021144,-0.135086418755761,
0.602991329634746));
#16261=CARTESIAN_POINT('Ctrl Pts',(0.0952657566843092,-0.101529863106778,
0.610933497757526));
#16262=CARTESIAN_POINT('Ctrl Pts',(0.136956022624868,0.025038477707157,
0.618875665880307));
#16263=CARTESIAN_POINT('Ctrl Pts',(0.0531805018142573,0.128669000640787,
0.626817834003085));
#16264=CARTESIAN_POINT('Ctrl Pts',(-0.0778376600742765,0.114584191752874,
0.634671515867523));
#16265=CARTESIAN_POINT('Ctrl Pts',(-0.117856827377429,0.0376798124439797,
0.639877808357699));
#16266=CARTESIAN_POINT('Ctrl Pts',(-0.117962383120995,-2.41598447144253E-5,
0.642436711473616));
#16267=CARTESIAN_POINT('Origin',(0.,0.,-0.0924367114736175));
#16268=CARTESIAN_POINT('',(-0.117934829819181,5.63106208242181E-5,0.532563288526383));
#16269=CARTESIAN_POINT('',(-0.117629301205424,7.34277634442948E-5,0.542436711473615));
#16270=CARTESIAN_POINT('',(-0.117775,2.85464118895969E-14,-0.0924367114736175));
#16271=CARTESIAN_POINT('Ctrl Pts',(-0.117934829819181,5.63106208242166E-5,
0.532563288526383));
#16272=CARTESIAN_POINT('Ctrl Pts',(-0.117723349859012,-0.0357608023914865,
0.534992624129852));
#16273=CARTESIAN_POINT('Ctrl Pts',(-0.0811985738067347,-0.110967619805887,
0.540068289612422));
#16274=CARTESIAN_POINT('Ctrl Pts',(0.0467759446245483,-0.131113145053959,
0.547790284974095));
#16275=CARTESIAN_POINT('Ctrl Pts',(0.135526478334676,-0.031799677225719,
0.555729274611401));
#16276=CARTESIAN_POINT('Ctrl Pts',(0.100211809365564,0.0966242157284558,
0.563668264248707));
#16277=CARTESIAN_POINT('Ctrl Pts',(-0.0268399031138932,0.136595261273209,
0.571607253886012));
#16278=CARTESIAN_POINT('Ctrl Pts',(-0.108142973925314,0.0691035501437442,
0.577905595311905));
#16279=CARTESIAN_POINT('Ctrl Pts',(-0.117708537635025,0.0149983997031143,
0.581557606858695));
#16280=CARTESIAN_POINT('Ctrl Pts',(-0.117626285855324,7.11112359239024E-5,
0.582563288526383));
#16281=CARTESIAN_POINT('Ctrl Pts',(-0.117629301205424,7.34277634442983E-5,
0.542436711473615));
#16282=CARTESIAN_POINT('Ctrl Pts',(-0.11748956090956,-0.0244625652698295,
0.544089858574172));
#16283=CARTESIAN_POINT('Ctrl Pts',(-0.0980201725405651,-0.0884941619373469,
0.548390395048989));
#16284=CARTESIAN_POINT('Ctrl Pts',(0.00702343738442799,-0.139048728244533,
0.555338320898066));
#16285=CARTESIAN_POINT('Ctrl Pts',(0.12066450826877,-0.0694546898587181,
0.563280489020846));
#16286=CARTESIAN_POINT('Ctrl Pts',(0.123764493242992,0.063766979789076,
0.571222657143626));
#16287=CARTESIAN_POINT('Ctrl Pts',(0.0134834875971477,0.13857154491934,
0.579164825266405));
#16288=CARTESIAN_POINT('Ctrl Pts',(-0.0957036897026042,0.092147346049863,
0.586236176709736));
#16289=CARTESIAN_POINT('Ctrl Pts',(-0.117475624432153,0.0262528025703711,
0.590660138778806));
#16290=CARTESIAN_POINT('Ctrl Pts',(-0.11766919235599,-9.26074537421669E-5,
0.592436711473616));
#16291=CARTESIAN_POINT('Origin',(0.,0.,-0.0924367114736175));
#16292=CARTESIAN_POINT('',(-0.117794891956694,-0.000106411733115368,0.482563288526384));
#16293=CARTESIAN_POINT('',(-0.117936566864074,5.52347650140707E-5,0.492436711473616));
#16294=CARTESIAN_POINT('',(-0.117775,2.85464118895969E-14,-0.0924367114736175));
#16295=CARTESIAN_POINT('Ctrl Pts',(-0.117794891956694,-0.000106411733115381,
0.482563288526384));
#16296=CARTESIAN_POINT('Ctrl Pts',(-0.117872998614688,-0.00856127641466401,
0.483134981642805));
#16297=CARTESIAN_POINT('Ctrl Pts',(-0.113184542395844,-0.0560672187853419,
0.486353004638329));
#16298=CARTESIAN_POINT('Ctrl Pts',(-0.0487302328423073,-0.130399425645183,
0.492217357512954));
#16299=CARTESIAN_POINT('Ctrl Pts',(0.0831353173341669,-0.111656458896056,
0.50015634715026));
#16300=CARTESIAN_POINT('Ctrl Pts',(0.13889618212661,0.00930034365552528,
0.508095336787567));
#16301=CARTESIAN_POINT('Ctrl Pts',(0.0675071113591811,0.12174331898465,
0.516034326424871));
#16302=CARTESIAN_POINT('Ctrl Pts',(-0.0656800932930844,0.122738629397884,
0.523973316062178));
#16303=CARTESIAN_POINT('Ctrl Pts',(-0.116384786286051,0.04545243224792,
0.529482970096015));
#16304=CARTESIAN_POINT('Ctrl Pts',(-0.117953719733239,0.00325558390455253,
0.53234629425075));
#16305=CARTESIAN_POINT('Ctrl Pts',(-0.117934829819181,5.63106208242166E-5,
0.532563288526383));
#16306=CARTESIAN_POINT('Ctrl Pts',(-0.117936566864074,5.52347650140663E-5,
0.492436711473616));
#16307=CARTESIAN_POINT('Ctrl Pts',(-0.117728017843002,-0.0358510361847084,
0.494872188995279));
#16308=CARTESIAN_POINT('Ctrl Pts',(-0.0810366231971402,-0.111156550628637,
0.499955055891203));
#16309=CARTESIAN_POINT('Ctrl Pts',(0.0471380885036503,-0.131003351527116,
0.507685312161385));
#16310=CARTESIAN_POINT('Ctrl Pts',(0.135643160584381,-0.031381690295376,
0.515627480284167));
#16311=CARTESIAN_POINT('Ctrl Pts',(0.0998851624184703,0.0969888232104648,
0.523569648406945));
#16312=CARTESIAN_POINT('Ctrl Pts',(-0.0273779061153799,0.136507610615132,
0.531511816529727));
#16313=CARTESIAN_POINT('Ctrl Pts',(-0.108290992649607,0.0687756007668377,
0.537800837551949));
#16314=CARTESIAN_POINT('Ctrl Pts',(-0.117713344367368,0.0148299618267192,
0.541442469199912));
#16315=CARTESIAN_POINT('Ctrl Pts',(-0.117629301205424,7.34277634442983E-5,
0.542436711473615));
#16316=CARTESIAN_POINT('Origin',(0.,0.,-0.0924367114736175));
#16317=CARTESIAN_POINT('',(-0.117582256074849,9.06819982020624E-6,0.432563288526383));
#16318=CARTESIAN_POINT('',(-0.11779560903417,-0.000106574656651148,0.442436711473616));
#16319=CARTESIAN_POINT('',(-0.117775,2.85464118895969E-14,-0.0924367114736175));
#16320=CARTESIAN_POINT('Ctrl Pts',(-0.117582256074849,9.06819982019261E-6,
0.432563288526383));
#16321=CARTESIAN_POINT('Ctrl Pts',(-0.117568373935691,-0.020201912089319,
0.43392366903486));
#16322=CARTESIAN_POINT('Ctrl Pts',(-0.10300922874285,-0.0797477867736473,
0.437930379422439));
#16323=CARTESIAN_POINT('Ctrl Pts',(-0.00838939967687663,-0.138954178686792,
0.44458341968912));
#16324=CARTESIAN_POINT('Ctrl Pts',(0.11219917790857,-0.0824013973067221,
0.452522409326426));
#16325=CARTESIAN_POINT('Ctrl Pts',(0.13007709763057,0.0495842159710775,
0.460461398963732));
#16326=CARTESIAN_POINT('Ctrl Pts',(0.0288783492374893,0.136178877755608,
0.468400388601037));
#16327=CARTESIAN_POINT('Ctrl Pts',(-0.0895654556576369,0.100852400902523,
0.475767685121922));
#16328=CARTESIAN_POINT('Ctrl Pts',(-0.117511448025972,0.0305757367622385,
0.480488651763704));
#16329=CARTESIAN_POINT('Ctrl Pts',(-0.117794891956694,-0.000106411733115381,
0.482563288526384));
#16330=CARTESIAN_POINT('Ctrl Pts',(-0.11779560903417,-0.000106574656651151,
0.442436711473616));
#16331=CARTESIAN_POINT('Ctrl Pts',(-0.117873644338608,-0.00854245500997505,
0.443007130042126));
#16332=CARTESIAN_POINT('Ctrl Pts',(-0.113196618671047,-0.056044542179559,
0.446224937984896));
#16333=CARTESIAN_POINT('Ctrl Pts',(-0.0487473834415776,-0.130413074907061,
0.452090135301926));
#16334=CARTESIAN_POINT('Ctrl Pts',(0.0831820848081396,-0.111645054821459,
0.460032303424706));
#16335=CARTESIAN_POINT('Ctrl Pts',(0.138908217753341,0.00940130521287039,
0.467974471547486));
#16336=CARTESIAN_POINT('Ctrl Pts',(0.0673801526530663,0.121835103839429,
0.475916639670265));
#16337=CARTESIAN_POINT('Ctrl Pts',(-0.0658750545035054,0.12265543075329,
0.483858807793047));
#16338=CARTESIAN_POINT('Ctrl Pts',(-0.116424939330292,0.0453161125527027,
0.489365498394162));
#16339=CARTESIAN_POINT('Ctrl Pts',(-0.11795471279604,0.00317945345687678,
0.492224799621019));
#16340=CARTESIAN_POINT('Ctrl Pts',(-0.117936566864074,5.52347650140663E-5,
0.492436711473616));
#16341=CARTESIAN_POINT('Origin',(0.,0.,-0.0924367114736175));
#16342=CARTESIAN_POINT('',(-0.117828183671793,0.000101754196006455,0.382563288526383));
#16343=CARTESIAN_POINT('',(-0.117581664177921,7.09484545444172E-6,0.392436711473616));
#16344=CARTESIAN_POINT('',(-0.117775,2.85464118895969E-14,-0.0924367114736175));
#16345=CARTESIAN_POINT('Ctrl Pts',(-0.117828183671793,0.000101754196006446,
0.382563288526384));
#16346=CARTESIAN_POINT('Ctrl Pts',(-0.117538790254565,-0.0316580736410773,
0.384712356426916));
#16347=CARTESIAN_POINT('Ctrl Pts',(-0.0879068326507716,-0.103002379129266,
0.38950775420655));
#16348=CARTESIAN_POINT('Ctrl Pts',(0.0326876424682324,-0.135315053971568,
0.396949481865287));
#16349=CARTESIAN_POINT('Ctrl Pts',(0.13141703692502,-0.0459152284901983,
0.404888471502591));
#16350=CARTESIAN_POINT('Ctrl Pts',(0.109843140674695,0.0855168418978295,
0.412827461139898));
#16351=CARTESIAN_POINT('Ctrl Pts',(-0.0122846228212416,0.13866410438033,
0.420766450777203));
#16352=CARTESIAN_POINT('Ctrl Pts',(-0.104166535924894,0.0775181589932739,
0.427345059906032));
#16353=CARTESIAN_POINT('Ctrl Pts',(-0.117595378674006,0.0191142356295008,
0.431277339155758));
#16354=CARTESIAN_POINT('Ctrl Pts',(-0.117582256074849,9.06819982019261E-6,
0.432563288526383));
#16355=CARTESIAN_POINT('Ctrl Pts',(-0.117581664177921,7.09484545444172E-6,
0.392436711473616));
#16356=CARTESIAN_POINT('Ctrl Pts',(-0.117570873504463,-0.0200907396801347,
0.393789460463232));
#16357=CARTESIAN_POINT('Ctrl Pts',(-0.10312708440739,-0.079535468422451,
0.397789598827109));
#16358=CARTESIAN_POINT('Ctrl Pts',(-0.00873482453528946,-0.138951719454826,
0.404437126565246));
#16359=CARTESIAN_POINT('Ctrl Pts',(0.112042812448737,-0.0826455423945668,
0.412379294688026));
#16360=CARTESIAN_POINT('Ctrl Pts',(0.130177722634257,0.049372441998279,
0.420321462810806));
#16361=CARTESIAN_POINT('Ctrl Pts',(0.0290564652212241,0.136160197297018,
0.428263630933586));
#16362=CARTESIAN_POINT('Ctrl Pts',(-0.0895090212855029,0.100936776489487,
0.435635380487856));
#16363=CARTESIAN_POINT('Ctrl Pts',(-0.117511471984497,0.0306096014671689,
0.440359740667866));
#16364=CARTESIAN_POINT('Ctrl Pts',(-0.11779560903417,-0.000106574656651151,
0.442436711473616));
#16365=CARTESIAN_POINT('Origin',(0.,0.,-0.0924367114736175));
#16366=CARTESIAN_POINT('',(-0.117911328466355,-7.22474488887591E-5,0.332563288526384));
#16367=CARTESIAN_POINT('',(-0.117821685414254,0.000103165543095151,0.342436711473616));
#16368=CARTESIAN_POINT('',(-0.117775,2.85464118895969E-14,-0.0924367114736175));
#16369=CARTESIAN_POINT('Ctrl Pts',(-0.117911328466355,-7.22474488887752E-5,
0.332563288526384));
#16370=CARTESIAN_POINT('Ctrl Pts',(-0.117942332027964,-0.00437115939612809,
0.332854713939869));
#16371=CARTESIAN_POINT('Ctrl Pts',(-0.115777752883067,-0.0476754067323583,
0.335792469232457));
#16372=CARTESIAN_POINT('Ctrl Pts',(-0.0622106591311991,-0.12453304658572,
0.341376554404146));
#16373=CARTESIAN_POINT('Ctrl Pts',(0.0708961914151981,-0.119801401679107,
0.349315544041452));
#16374=CARTESIAN_POINT('Ctrl Pts',(0.1391024375543,-0.00539978406154301,
0.357254533678757));
#16375=CARTESIAN_POINT('Ctrl Pts',(0.0799699354250877,0.113944965792994,
0.365193523316063));
#16376=CARTESIAN_POINT('Ctrl Pts',(-0.0523695618881846,0.128980908622551,
0.373132512953369));
#16377=CARTESIAN_POINT('Ctrl Pts',(-0.113921748517257,0.0538356345748906,
0.378922434690143));
#16378=CARTESIAN_POINT('Ctrl Pts',(-0.117895144954496,0.00745050051778832,
0.382066026547814));
#16379=CARTESIAN_POINT('Ctrl Pts',(-0.117828183671793,0.000101754196006446,
0.382563288526384));
#16380=CARTESIAN_POINT('Ctrl Pts',(-0.117821685414254,0.000103165543095145,
0.342436711473616));
#16381=CARTESIAN_POINT('Ctrl Pts',(-0.117532262555972,-0.0314544122979593,
0.344571790884339));
#16382=CARTESIAN_POINT('Ctrl Pts',(-0.0882170202347594,-0.102616110661261,
0.349354259669323));
#16383=CARTESIAN_POINT('Ctrl Pts',(0.0320320385160992,-0.135491055083419,
0.356784117828566));
#16384=CARTESIAN_POINT('Ctrl Pts',(0.131227975626944,-0.0465090949381858,
0.364726285951346));
#16385=CARTESIAN_POINT('Ctrl Pts',(0.110205605501345,0.0850799742312894,
0.372668454074126));
#16386=CARTESIAN_POINT('Ctrl Pts',(-0.0117764211155082,0.138727046407055,
0.380610622196906));
#16387=CARTESIAN_POINT('Ctrl Pts',(-0.10403099481448,0.0777947493501838,
0.387200041330069));
#16388=CARTESIAN_POINT('Ctrl Pts',(-0.117591991327853,0.019241607989002,
0.391142071088973));
#16389=CARTESIAN_POINT('Ctrl Pts',(-0.117581664177921,7.09484545444172E-6,
0.392436711473616));
#16390=CARTESIAN_POINT('Origin',(0.,0.,-0.0924367114736175));
#16391=CARTESIAN_POINT('',(-0.117608153246896,-5.64262068778628E-5,0.282563288526383));
#16392=CARTESIAN_POINT('',(-0.117918861549493,-6.80329776671096E-5,0.292436711473615));
#16393=CARTESIAN_POINT('',(-0.117775,2.85464118895969E-14,-0.0924367114736175));
#16394=CARTESIAN_POINT('Ctrl Pts',(-0.117608153246896,-5.64262068778604E-5,
0.282563288526383));
#16395=CARTESIAN_POINT('Ctrl Pts',(-0.117677606263852,-0.0160946837114709,
0.283643401331924));
#16396=CARTESIAN_POINT('Ctrl Pts',(-0.107144424846824,-0.0713401098021974,
0.287369844016567));
#16397=CARTESIAN_POINT('Ctrl Pts',(-0.0229969941138309,-0.137294515779738,
0.293742616580312));
#16398=CARTESIAN_POINT('Ctrl Pts',(0.102883268653204,-0.0937746172089793,
0.301681606217617));
#16399=CARTESIAN_POINT('Ctrl Pts',(0.134580950019115,0.0355895166223291,
0.309620595854923));
#16400=CARTESIAN_POINT('Ctrl Pts',(0.0430789950773988,0.13237388709478,
0.317559585492229));
#16401=CARTESIAN_POINT('Ctrl Pts',(-0.0830523456774332,0.10887452531409,
0.325207149716049));
#16402=CARTESIAN_POINT('Ctrl Pts',(-0.11766079978112,0.0346657214219864,
0.330208384060767));
#16403=CARTESIAN_POINT('Ctrl Pts',(-0.117911328466355,-7.22474488887752E-5,
0.332563288526384));
#16404=CARTESIAN_POINT('Ctrl Pts',(-0.117918861549493,-6.80329776671157E-5,
0.292436711473616));
#16405=CARTESIAN_POINT('Ctrl Pts',(-0.117946256357307,-0.00405052459867665,
0.292706731931186));
#16406=CARTESIAN_POINT('Ctrl Pts',(-0.11595553950755,-0.0470512577090033,
0.295624141763016));
#16407=CARTESIAN_POINT('Ctrl Pts',(-0.0631725212350128,-0.124068972994571,
0.301188940969106));
#16408=CARTESIAN_POINT('Ctrl Pts',(0.0700327441786229,-0.12032993078169,
0.309131109091886));
#16409=CARTESIAN_POINT('Ctrl Pts',(0.139080821187468,-0.00635631000930847,
0.317073277214666));
#16410=CARTESIAN_POINT('Ctrl Pts',(0.0807165776729536,0.11344034374014,
0.325015445337446));
#16411=CARTESIAN_POINT('Ctrl Pts',(-0.0515923433190751,0.129313988454311,
0.332957613460226));
#16412=CARTESIAN_POINT('Ctrl Pts',(-0.113774867115171,0.0543021652640841,
0.338764702172283));
#16413=CARTESIAN_POINT('Ctrl Pts',(-0.117891132111753,0.00767537174388221,
0.341924401510079));
#16414=CARTESIAN_POINT('Ctrl Pts',(-0.117821685414254,0.000103165543095145,
0.342436711473616));
#16415=CARTESIAN_POINT('Origin',(0.,0.,-0.0924367114736175));
#16416=CARTESIAN_POINT('',(-0.117705188630573,0.000102098618198066,0.232563288526383));
#16417=CARTESIAN_POINT('',(-0.1176142238744,-6.23262858038681E-5,0.242436711473616));
#16418=CARTESIAN_POINT('',(-0.117775,2.85464118895969E-14,-0.0924367114736175));
#16419=CARTESIAN_POINT('Ctrl Pts',(-0.117705188630573,0.000102098618198071,
0.232563288526383));
#16420=CARTESIAN_POINT('Ctrl Pts',(-0.117475649963863,-0.0275896003179174,
0.234432088723979));
#16421=CARTESIAN_POINT('Ctrl Pts',(-0.0938913217252411,-0.0948462909608301,
0.238947218800678));
#16422=CARTESIAN_POINT('Ctrl Pts',(0.0182347644767634,-0.138007750384372,
0.246108678756477));
#16423=CARTESIAN_POINT('Ctrl Pts',(0.125841858853055,-0.0595186723796334,
0.254047668393783));
#16424=CARTESIAN_POINT('Ctrl Pts',(0.118249355954961,0.073455671106145,
0.261986658031089));
#16425=CARTESIAN_POINT('Ctrl Pts',(0.00240767183786234,0.139186381940956,
0.269925647668394));
#16426=CARTESIAN_POINT('Ctrl Pts',(-0.0995777503027144,0.0858938305448248,
0.27678452450016));
#16427=CARTESIAN_POINT('Ctrl Pts',(-0.117507442931816,0.0231998416616275,
0.280997071452822));
#16428=CARTESIAN_POINT('Ctrl Pts',(-0.117608153246896,-5.64262068778604E-5,
0.282563288526383));
#16429=CARTESIAN_POINT('Ctrl Pts',(-0.1176142238744,-6.2326285803882E-5,
0.242436711473616));
#16430=CARTESIAN_POINT('Ctrl Pts',(-0.117689148257971,-0.0156863246439697,
0.243489062352292));
#16431=CARTESIAN_POINT('Ctrl Pts',(-0.107519643382358,-0.0705218816827611,
0.247188802605229));
#16432=CARTESIAN_POINT('Ctrl Pts',(-0.024381182195918,-0.137074561658528,
0.253535932232426));
#16433=CARTESIAN_POINT('Ctrl Pts',(0.101985705091022,-0.094777599970642,
0.261478100355206));
#16434=CARTESIAN_POINT('Ctrl Pts',(0.134923209124943,0.0343453801629359,
0.269420268477986));
#16435=CARTESIAN_POINT('Ctrl Pts',(0.0442571924125319,0.132004463632409,
0.277362436600766));
#16436=CARTESIAN_POINT('Ctrl Pts',(-0.0824920331482911,0.109525057495754,
0.285034584265976));
#16437=CARTESIAN_POINT('Ctrl Pts',(-0.117677666622401,0.0349954280503056,
0.290059342556926));
#16438=CARTESIAN_POINT('Ctrl Pts',(-0.117918861549493,-6.80329776671157E-5,
0.292436711473616));
#16439=CARTESIAN_POINT('Origin',(0.,0.,-0.0924367114736175));
#16440=CARTESIAN_POINT('',(-0.117967994073432,-3.0724305424694E-6,0.182563288526383));
#16441=CARTESIAN_POINT('',(-0.117691121003631,9.91971943564221E-5,0.192436711473615));
#16442=CARTESIAN_POINT('',(-0.117775,2.85464118895969E-14,-0.0924367114736175));
#16443=CARTESIAN_POINT('Ctrl Pts',(-0.117967994073432,-3.07243054247449E-6,
0.182563288526383));
#16444=CARTESIAN_POINT('Ctrl Pts',(-0.117968057042159,-0.000167453844217198,
0.182574446236933));
#16445=CARTESIAN_POINT('Ctrl Pts',(-0.117893299674953,-0.0393189363008842,
0.185231933826584));
#16446=CARTESIAN_POINT('Ctrl Pts',(-0.0749972298318695,-0.11727771015962,
0.190535751295337));
#16447=CARTESIAN_POINT('Ctrl Pts',(0.0578663373665801,-0.126610160769685,
0.198474740932643));
#16448=CARTESIAN_POINT('Ctrl Pts',(0.13775723856723,-0.0200396862227523,
0.206413730569949));
#16449=CARTESIAN_POINT('Ctrl Pts',(0.091540828968026,0.104875747581476,
0.214352720207254));
#16450=CARTESIAN_POINT('Ctrl Pts',(-0.0384749358425138,0.133784622116252,
0.22229170984456));
#16451=CARTESIAN_POINT('Ctrl Pts',(-0.110955338697302,0.0622468391270206,
0.22836189928427));
#16452=CARTESIAN_POINT('Ctrl Pts',(-0.11780069007939,0.0116234575531164,
0.231785758844877));
#16453=CARTESIAN_POINT('Ctrl Pts',(-0.117705188630573,0.000102098618198071,
0.232563288526383));
#16454=CARTESIAN_POINT('Ctrl Pts',(-0.117691121003631,9.91971943564221E-5,
0.192436711473615));
#16455=CARTESIAN_POINT('Ctrl Pts',(-0.117474218986382,-0.0270951350261672,
0.194271392773399));
#16456=CARTESIAN_POINT('Ctrl Pts',(-0.0945676524372527,-0.0938598508209937,
0.198753463447442));
#16457=CARTESIAN_POINT('Ctrl Pts',(0.0165156171993534,-0.138242945169174,
0.205882923495746));
#16458=CARTESIAN_POINT('Ctrl Pts',(0.125131592687617,-0.061040658666823,
0.213825091618526));
#16459=CARTESIAN_POINT('Ctrl Pts',(0.119114174013628,0.0720811421096423,
0.221767259741306));
#16460=CARTESIAN_POINT('Ctrl Pts',(0.0039759348809324,0.139169211541763,
0.229709427864086));
#16461=CARTESIAN_POINT('Ctrl Pts',(-0.0990660356104632,0.0867677816679632,
0.236599245108189));
#16462=CARTESIAN_POINT('Ctrl Pts',(-0.117500661679058,0.0236188235484957,
0.240841672978032));
#16463=CARTESIAN_POINT('Ctrl Pts',(-0.1176142238744,-6.2326285803882E-5,
0.242436711473616));
#16464=CARTESIAN_POINT('Origin',(0.,0.,-0.0924367114736175));
#16465=CARTESIAN_POINT('',(-0.117696212882312,-0.000100181105204699,0.132563288526383));
#16466=CARTESIAN_POINT('',(-0.117967699956222,8.3697257429456E-6,0.142436711473616));
#16467=CARTESIAN_POINT('',(-0.117775,2.85464118895969E-14,-0.0924367114736175));
#16468=CARTESIAN_POINT('Ctrl Pts',(-0.117696212882312,-0.000100181105204706,
0.132563288526383));
#16469=CARTESIAN_POINT('Ctrl Pts',(-0.117792074781153,-0.0119544960022407,
0.133363133628988));
#16470=CARTESIAN_POINT('Ctrl Pts',(-0.110696412003459,-0.0629173266909915,
0.136809308610694));
#16471=CARTESIAN_POINT('Ctrl Pts',(-0.0373480950846616,-0.134103559412242,
0.142901813471503));
#16472=CARTESIAN_POINT('Ctrl Pts',(0.0924198687735613,-0.104101940294199,
0.150840803108809));
#16473=CARTESIAN_POINT('Ctrl Pts',(0.137583777756591,0.0211978768359354,
0.158779792746114));
#16474=CARTESIAN_POINT('Ctrl Pts',(0.0567991668878991,0.127092487218924,
0.16671878238342));
#16475=CARTESIAN_POINT('Ctrl Pts',(-0.0757945745091616,0.116657324056303,
0.174646614310176));
#16476=CARTESIAN_POINT('Ctrl Pts',(-0.117953122434976,0.0388197061692436,
0.179928116357831));
#16477=CARTESIAN_POINT('Ctrl Pts',(-0.117967994073432,-3.07243054247449E-6,
0.182563288526383));
#16478=CARTESIAN_POINT('Ctrl Pts',(-0.117967699956222,8.3697257429579E-6,
0.142436711473616));
#16479=CARTESIAN_POINT('Ctrl Pts',(-0.117928252023989,-0.038547130539091,
0.145053723194506));
#16480=CARTESIAN_POINT('Ctrl Pts',(-0.0762804946418446,-0.116178754198862,
0.150318124289656));
#16481=CARTESIAN_POINT('Ctrl Pts',(0.0559861945572589,-0.127473226882309,
0.158229914759066));
#16482=CARTESIAN_POINT('Ctrl Pts',(0.137471621702818,-0.0220324926503626,
0.166172082881846));
#16483=CARTESIAN_POINT('Ctrl Pts',(0.0930189202108026,0.103592267873211,
0.174114251004626));
#16484=CARTESIAN_POINT('Ctrl Pts',(-0.0366486683060043,0.134315868829211,
0.182056419127406));
#16485=CARTESIAN_POINT('Ctrl Pts',(-0.110544190454925,0.0633195416932908,
0.188163905950403));
#16486=CARTESIAN_POINT('Ctrl Pts',(-0.11778720200735,0.0121454601492482,
0.191624003399139));
#16487=CARTESIAN_POINT('Ctrl Pts',(-0.117691121003631,9.91971943564221E-5,
0.192436711473615));
#16488=CARTESIAN_POINT('Origin',(0.,0.,-0.0924367114736175));
#16489=CARTESIAN_POINT('',(-0.117613109409711,6.11591708146705E-5,0.0825632885263832));
#16490=CARTESIAN_POINT('',(-0.117715749944134,-0.000104199409386274,0.0924367114736155));
#16491=CARTESIAN_POINT('',(-0.117775,2.85464118895969E-14,-0.0924367114736175));
#16492=CARTESIAN_POINT('Ctrl Pts',(-0.117613109409711,6.11591708146765E-5,
0.0825632885263832));
#16493=CARTESIAN_POINT('Ctrl Pts',(-0.117502393620717,-0.0235240259785673,
0.0841518210210431));
#16494=CARTESIAN_POINT('Ctrl Pts',(-0.0991849320095013,-0.0865581493706475,
0.088386683394805));
#16495=CARTESIAN_POINT('Ctrl Pts',(0.00357853460314598,-0.139161043603659,
0.0952678756476685));
#16496=CARTESIAN_POINT('Ctrl Pts',(0.118863112008681,-0.0724583686054966,
0.103206865284975));
#16497=CARTESIAN_POINT('Ctrl Pts',(0.125336705278751,0.0605752693714656,
0.11114585492228));
#16498=CARTESIAN_POINT('Ctrl Pts',(0.0170731091066207,0.138156245709763,
0.119084844559586));
#16499=CARTESIAN_POINT('Ctrl Pts',(-0.094337657277608,0.0941904991302726,
0.126223989094287));
#16500=CARTESIAN_POINT('Ctrl Pts',(-0.11747491061231,0.0272661325996615,
0.130716803749886));
#16501=CARTESIAN_POINT('Ctrl Pts',(-0.117696212882312,-0.000100181105204706,
0.132563288526383));
#16502=CARTESIAN_POINT('Ctrl Pts',(-0.117715749944134,-0.000104199409386274,
0.0924367114736155));
#16503=CARTESIAN_POINT('Ctrl Pts',(-0.117810584636384,-0.011244028442556,
0.0931886642413524));
#16504=CARTESIAN_POINT('Ctrl Pts',(-0.111246641208053,-0.0614941526881817,
0.0965880063833492));
#16505=CARTESIAN_POINT('Ctrl Pts',(-0.0397151780004399,-0.133441281507892,
0.102634737899606));
#16506=CARTESIAN_POINT('Ctrl Pts',(0.0906220264938673,-0.105695447092796,
0.110576906022386));
#16507=CARTESIAN_POINT('Ctrl Pts',(0.137940159127448,0.0188783162799928,
0.118519074145166));
#16508=CARTESIAN_POINT('Ctrl Pts',(0.0588909273047484,0.126157580947307,
0.126461242267946));
#16509=CARTESIAN_POINT('Ctrl Pts',(-0.074108440039672,0.117863552156501,
0.134403410390726));
#16510=CARTESIAN_POINT('Ctrl Pts',(-0.117763087033452,0.0399060678969832,
0.139728566792616));
#16511=CARTESIAN_POINT('Ctrl Pts',(-0.117968157858494,0.000455912857932787,
0.142406333820246));
#16512=CARTESIAN_POINT('Ctrl Pts',(-0.117967699956222,8.3697257429579E-6,
0.142436711473616));
#16513=CARTESIAN_POINT('Origin',(0.,0.,-0.0924367114736175));
#16514=CARTESIAN_POINT('',(-0.117917485785546,7.60014832213593E-5,0.0325632885263832));
#16515=CARTESIAN_POINT('',(-0.117600989619072,5.04992496179954E-5,0.0424367114736154));
#16516=CARTESIAN_POINT('',(-0.117775,2.85464118895969E-14,-0.0924367114736175));
#16517=CARTESIAN_POINT('Ctrl Pts',(-0.117917485785546,7.60014832213644E-5,
0.0325632885263832));
#16518=CARTESIAN_POINT('Ctrl Pts',(-0.117676727567847,-0.0349830640657269,
0.0349405084130983));
#16519=CARTESIAN_POINT('Ctrl Pts',(-0.0825043195215805,-0.109517225708346,
0.0399640581789154));
#16520=CARTESIAN_POINT('Ctrl Pts',(0.0441923146003338,-0.131999388615902,
0.0476339378238343));
#16521=CARTESIAN_POINT('Ctrl Pts',(0.134874939024977,-0.034459980695041,
0.0555729274611401));
#16522=CARTESIAN_POINT('Ctrl Pts',(0.102091080224759,0.094638871230671,
0.0635119170984456));
#16523=CARTESIAN_POINT('Ctrl Pts',(-0.0241513666277066,0.137095110112719,
0.0714509067357516));
#16524=CARTESIAN_POINT('Ctrl Pts',(-0.107448046275642,0.0706698818446754,
0.0778013638783972));
#16525=CARTESIAN_POINT('Ctrl Pts',(-0.117686834607281,0.0157664388843013,
0.0815054911419412));
#16526=CARTESIAN_POINT('Ctrl Pts',(-0.117613109409711,6.11591708146765E-5,
0.0825632885263832));
#16527=CARTESIAN_POINT('Ctrl Pts',(-0.117600989619072,5.04992496179954E-5,
0.0424367114736154));
#16528=CARTESIAN_POINT('Ctrl Pts',(-0.117514779739531,-0.0227353060542692,
0.043970994662459));
#16529=CARTESIAN_POINT('Ctrl Pts',(-0.100129952091853,-0.0849605109884783,
0.0481526672255625));
#16530=CARTESIAN_POINT('Ctrl Pts',(0.000787973702835166,-0.139222729671589,
0.054981729162926));
#16531=CARTESIAN_POINT('Ctrl Pts',(0.117431922513572,-0.0747907597173192,
0.0629238972857061));
#16532=CARTESIAN_POINT('Ctrl Pts',(0.126496838785129,0.0581591461343325,
0.070866065408486));
#16533=CARTESIAN_POINT('Ctrl Pts',(0.0196773008918215,0.137828289815661,
0.0788082335312661));
#16534=CARTESIAN_POINT('Ctrl Pts',(-0.0933482651079043,0.0956446566614129,
0.085998448886309));
#16535=CARTESIAN_POINT('Ctrl Pts',(-0.11747670148927,0.0279758085988667,
0.0905412748670923));
#16536=CARTESIAN_POINT('Ctrl Pts',(-0.117715749944134,-0.000104199409386274,
0.0924367114736155));
#16537=CARTESIAN_POINT('Origin',(0.,0.,1.55));
#16538=CARTESIAN_POINT('',(-0.143211704627722,-5.70397197726547E-6,1.50700023576178));
#16539=CARTESIAN_POINT('Ctrl Pts',(-0.0334019664626774,0.112939183906323,
1.532225));
#16540=CARTESIAN_POINT('Ctrl Pts',(-0.0250606930336426,0.115799676338094,
1.53184761307169));
#16541=CARTESIAN_POINT('Ctrl Pts',(-0.0164287086124659,0.117635554524944,
1.53147359869818));
#16542=CARTESIAN_POINT('Ctrl Pts',(-0.00767226928320402,0.118510614220874,
1.53110056493424));
#16543=CARTESIAN_POINT('Ctrl Pts',(-0.0042150196872779,0.118856108509867,
1.53095328237096));
#16544=CARTESIAN_POINT('Ctrl Pts',(-0.000736351480830917,0.119051293525916,
1.53080607672538));
#16545=CARTESIAN_POINT('Ctrl Pts',(0.00274830211697625,0.119097943881266,
1.53065904037218));
#16546=CARTESIAN_POINT('Ctrl Pts',(0.00972321854123044,0.119191319684798,
1.53036473098213));
#16547=CARTESIAN_POINT('Ctrl Pts',(0.0166907125456733,0.118690968429664,
1.53007241075126));
#16548=CARTESIAN_POINT('Ctrl Pts',(0.0235721318645625,0.11762150546261,
1.52978094357425));
#16549=CARTESIAN_POINT('Ctrl Pts',(0.0273478463565568,0.117034709826966,
1.52962102062912));
#16550=CARTESIAN_POINT('Ctrl Pts',(0.0310977188904398,0.116276259986281,
1.52946135449799));
#16551=CARTESIAN_POINT('Ctrl Pts',(0.0348087249896146,0.115347945392283,
1.52930175751644));
#16552=CARTESIAN_POINT('Ctrl Pts',(0.0378768737129624,0.114580442682688,
1.52916980751093));
#16553=CARTESIAN_POINT('Ctrl Pts',(0.0409182562642153,0.113696477767379,
1.52903790896105));
#16554=CARTESIAN_POINT('Ctrl Pts',(0.0439120268522727,0.112701821307647,
1.52890655030309));
#16555=CARTESIAN_POINT('Ctrl Pts',(0.0504861734289241,0.110517613410832,
1.52861809430882));
#16556=CARTESIAN_POINT('Ctrl Pts',(0.0568477403450367,0.107796947733889,
1.528331525126));
#16557=CARTESIAN_POINT('Ctrl Pts',(0.0629211062797432,0.10455513280498,
1.52804576869741));
#16558=CARTESIAN_POINT('Ctrl Pts',(0.0667529140263229,0.102509807084265,
1.52786547926507));
#16559=CARTESIAN_POINT('Ctrl Pts',(0.0704699809867569,0.100256700264741,
1.52768551335768));
#16560=CARTESIAN_POINT('Ctrl Pts',(0.0740519796445933,0.0977963961590643,
1.52750560123222));
#16561=CARTESIAN_POINT('Ctrl Pts',(0.0761474027326905,0.0963571499395001,
1.52740035495562));
#16562=CARTESIAN_POINT('Ctrl Pts',(0.0781972522873126,0.0948464165467323,
1.52729509152825));
#16563=CARTESIAN_POINT('Ctrl Pts',(0.0801950758490376,0.0932655888959708,
1.52718986717129));
#16564=CARTESIAN_POINT('Ctrl Pts',(0.0872135629190184,0.0877120362002772,
1.52682020700562));
#16565=CARTESIAN_POINT('Ctrl Pts',(0.0935342345834078,0.0813437113039547,
1.52645409167081));
#16566=CARTESIAN_POINT('Ctrl Pts',(0.0991216768718319,0.0743433873765979,
1.52608928877518));
#16567=CARTESIAN_POINT('Ctrl Pts',(0.101857856375295,0.0709153174549959,
1.52591064420861));
#16568=CARTESIAN_POINT('Ctrl Pts',(0.104417791592617,0.0673349702414553,
1.52573231437502));
#16569=CARTESIAN_POINT('Ctrl Pts',(0.106794530290299,0.0636205708890664,
1.52555403711528));
#16570=CARTESIAN_POINT('Ctrl Pts',(0.108394385735532,0.0611202951812291,
1.52543403324399));
#16571=CARTESIAN_POINT('Ctrl Pts',(0.109912312880749,0.0585571637778213,
1.52531395827658));
#16572=CARTESIAN_POINT('Ctrl Pts',(0.111341951189028,0.0559432008961949,
1.5251940432238));
#16573=CARTESIAN_POINT('Ctrl Pts',(0.115894033640165,0.0476201345006791,
1.52481222412716));
#16574=CARTESIAN_POINT('Ctrl Pts',(0.119530893641226,0.0388304356906876,
1.52443409356659));
#16575=CARTESIAN_POINT('Ctrl Pts',(0.122195159250079,0.0297595052710396,
1.52405718851832));
#16576=CARTESIAN_POINT('Ctrl Pts',(0.123464283518865,0.0254385629829291,
1.52387764960816));
#16577=CARTESIAN_POINT('Ctrl Pts',(0.124512110981915,0.0210533134598664,
1.52369838877875));
#16578=CARTESIAN_POINT('Ctrl Pts',(0.12532867129748,0.0166220814218575,
1.52351913980531));
#16579=CARTESIAN_POINT('Ctrl Pts',(0.126067828800149,0.012610891624201,
1.52335688207487));
#16580=CARTESIAN_POINT('Ctrl Pts',(0.12661735951473,0.00855739899605222,
1.52319445303817));
#16581=CARTESIAN_POINT('Ctrl Pts',(0.126966826155483,0.00450415768051923,
1.52303280899981));
#16582=CARTESIAN_POINT('Ctrl Pts',(0.127602972227412,-0.00287409603749457,
1.52273856283131));
#16583=CARTESIAN_POINT('Ctrl Pts',(0.12758177643555,-0.010267620141741,
1.52244625042084));
#16584=CARTESIAN_POINT('Ctrl Pts',(0.126865581413421,-0.0175939782534482,
1.52215473434257));
#16585=CARTESIAN_POINT('Ctrl Pts',(0.126426462283551,-0.0220859726121444,
1.52197599770985));
#16586=CARTESIAN_POINT('Ctrl Pts',(0.12572570473317,-0.0265528301690258,
1.52179756043894));
#16587=CARTESIAN_POINT('Ctrl Pts',(0.124776542651163,-0.0309793260681717,
1.52161916036391));
#16588=CARTESIAN_POINT('Ctrl Pts',(0.124151644840291,-0.0338935887106027,
1.52150170748789));
#16589=CARTESIAN_POINT('Ctrl Pts',(0.123418330834614,-0.0367926408403149,
1.52138417707714));
#16590=CARTESIAN_POINT('Ctrl Pts',(0.122581975874549,-0.0396644408336013,
1.52126680258073));
#16591=CARTESIAN_POINT('Ctrl Pts',(0.120074191833131,-0.0482754427851461,
1.52091485884509));
#16592=CARTESIAN_POINT('Ctrl Pts',(0.116656903439717,-0.0566007293654626,
1.52056600333313));
#16593=CARTESIAN_POINT('Ctrl Pts',(0.112443760417108,-0.0645262187619275,
1.52021830866717));
#16594=CARTESIAN_POINT('Ctrl Pts',(0.109356904590302,-0.0703330102694749,
1.51996356219884));
#16595=CARTESIAN_POINT('Ctrl Pts',(0.105841781173658,-0.0759253337267248,
1.51970943888381));
#16596=CARTESIAN_POINT('Ctrl Pts',(0.101930367117466,-0.0812537151913617,
1.51945518067311));
#16597=CARTESIAN_POINT('Ctrl Pts',(0.100130771446666,-0.0837052409256295,
1.51933819945644));
#16598=CARTESIAN_POINT('Ctrl Pts',(0.0982476276828181,-0.0860996963839449,
1.51922123442864));
#16599=CARTESIAN_POINT('Ctrl Pts',(0.0962924325256194,-0.0884227179472683,
1.51910469697823));
#16600=CARTESIAN_POINT('Ctrl Pts',(0.0906946176521128,-0.0950736369671782,
1.51877104482549));
#16601=CARTESIAN_POINT('Ctrl Pts',(0.0844921899154374,-0.101162815315101,
1.51843983772287));
#16602=CARTESIAN_POINT('Ctrl Pts',(0.0777644521522082,-0.106582693579069,
1.51810941878));
#16603=CARTESIAN_POINT('Ctrl Pts',(0.0731067700043679,-0.110334931124879,
1.5178806663426));
#16604=CARTESIAN_POINT('Ctrl Pts',(0.0681966627772886,-0.113766151308436,
1.51765229166508));
#16605=CARTESIAN_POINT('Ctrl Pts',(0.0630541948599911,-0.116833686038022,
1.5174237449583));
#16606=CARTESIAN_POINT('Ctrl Pts',(0.0607686815400033,-0.118197018118406,
1.51732216988754));
#16607=CARTESIAN_POINT('Ctrl Pts',(0.0584414404741937,-0.119485783651375,
1.51722075040181));
#16608=CARTESIAN_POINT('Ctrl Pts',(0.0560784264268894,-0.12069488199044,
1.51711960151386));
#16609=CARTESIAN_POINT('Ctrl Pts',(0.0475595529450054,-0.125053787850271,
1.51675495087613));
#16610=CARTESIAN_POINT('Ctrl Pts',(0.038563113830939,-0.128389854466075,
1.51639315730301));
#16611=CARTESIAN_POINT('Ctrl Pts',(0.0292711048986314,-0.130741856378471,
1.51603205677802));
#16612=CARTESIAN_POINT('Ctrl Pts',(0.0254547302664753,-0.13170786066222,
1.51588374709674));
#16613=CARTESIAN_POINT('Ctrl Pts',(0.0215881861914954,-0.132507324978224,
1.51573555432397));
#16614=CARTESIAN_POINT('Ctrl Pts',(0.0176832233642019,-0.13314066674995,
1.51558732853105));
#16615=CARTESIAN_POINT('Ctrl Pts',(0.0144414794405867,-0.133666441752394,
1.51546427740745));
#16616=CARTESIAN_POINT('Ctrl Pts',(0.0111713231872828,-0.134077605234841,
1.5153411329761));
#16617=CARTESIAN_POINT('Ctrl Pts',(0.00789687394913892,-0.134372952697723,
1.51521845803943));
#16618=CARTESIAN_POINT('Ctrl Pts',(-0.00208492598009478,-0.135273287095873,
1.51484449692866));
#16619=CARTESIAN_POINT('Ctrl Pts',(-0.0121386692885745,-0.135107999768821,
1.51447364169918));
#16620=CARTESIAN_POINT('Ctrl Pts',(-0.0220717676774029,-0.133899092645375,
1.51410356562093));
#16621=CARTESIAN_POINT('Ctrl Pts',(-0.0271373055616968,-0.133282591671289,
1.51391483957382));
#16622=CARTESIAN_POINT('Ctrl Pts',(-0.0321716696217597,-0.132393849601707,
1.51372631615657));
#16623=CARTESIAN_POINT('Ctrl Pts',(-0.0371491047637803,-0.131230566976147,
1.51353768678866));
#16624=CARTESIAN_POINT('Ctrl Pts',(-0.0401763453142056,-0.130523066780721,
1.51342296375255));
#16625=CARTESIAN_POINT('Ctrl Pts',(-0.0431793745847511,-0.129714439573166,
1.51330831773957));
#16626=CARTESIAN_POINT('Ctrl Pts',(-0.0461427198170546,-0.128807808452418,
1.51319405707679));
#16627=CARTESIAN_POINT('Ctrl Pts',(-0.0557912886485991,-0.125855842991896,
1.51282202756853));
#16628=CARTESIAN_POINT('Ctrl Pts',(-0.0650506639775802,-0.121862017750276,
1.51245293010828));
#16629=CARTESIAN_POINT('Ctrl Pts',(-0.0737251756215706,-0.116823260910032,
1.51208446868514));
#16630=CARTESIAN_POINT('Ctrl Pts',(-0.0774533877539874,-0.114657657224767,
1.51192610791459));
#16631=CARTESIAN_POINT('Ctrl Pts',(-0.0810733781510443,-0.112298364258586,
1.51176786463208));
#16632=CARTESIAN_POINT('Ctrl Pts',(-0.0845783705992567,-0.109758519633299,
1.51160955655689));
#16633=CARTESIAN_POINT('Ctrl Pts',(-0.0871260289206952,-0.107912394030924,
1.51149448786814));
#16634=CARTESIAN_POINT('Ctrl Pts',(-0.0896122610481647,-0.105970921032248,
1.51137940572563));
#16635=CARTESIAN_POINT('Ctrl Pts',(-0.0920243025666997,-0.10394826075131,
1.51126473391974));
#16636=CARTESIAN_POINT('Ctrl Pts',(-0.0995315444015674,-0.0976529296958118,
1.51090782920982));
#16637=CARTESIAN_POINT('Ctrl Pts',(-0.106349817996106,-0.090554906599088,
1.51055366538392));
#16638=CARTESIAN_POINT('Ctrl Pts',(-0.112409916721278,-0.0828189535999138,
1.51020021897155));
#16639=CARTESIAN_POINT('Ctrl Pts',(-0.11567060314877,-0.0786565598680515,
1.51001004419521));
#16640=CARTESIAN_POINT('Ctrl Pts',(-0.118711357121208,-0.0743087544864998,
1.50982007711492));
#16641=CARTESIAN_POINT('Ctrl Pts',(-0.121517490738653,-0.0697974244982526,
1.50963000253165));
#16642=CARTESIAN_POINT('Ctrl Pts',(-0.123184827969132,-0.0671169005197731,
1.50951706477726));
#16643=CARTESIAN_POINT('Ctrl Pts',(-0.124768226583796,-0.064379797453554,
1.50940414472167));
#16644=CARTESIAN_POINT('Ctrl Pts',(-0.12625918933752,-0.0616017405091787,
1.50929161182319));
#16645=CARTESIAN_POINT('Ctrl Pts',(-0.131254477666307,-0.0522942005345653,
1.50891458411209));
#16646=CARTESIAN_POINT('Ctrl Pts',(-0.135235816373665,-0.0424980109473837,
1.50854057440173));
#16647=CARTESIAN_POINT('Ctrl Pts',(-0.138100316247284,-0.0323932585971084,
1.50816719719795));
#16648=CARTESIAN_POINT('Ctrl Pts',(-0.139428601593765,-0.027707625827389,
1.5079940600046));
#16649=CARTESIAN_POINT('Ctrl Pts',(-0.140516076092011,-0.0229552175461711,
1.50782105881478));
#16650=CARTESIAN_POINT('Ctrl Pts',(-0.14134846970832,-0.01815262603916,
1.50764795577689));
#16651=CARTESIAN_POINT('Ctrl Pts',(-0.141840021659925,-0.0153165600461233,
1.5075457335416));
#16652=CARTESIAN_POINT('Ctrl Pts',(-0.142241997144177,-0.0124651428186592,
1.50744355431084));
#16653=CARTESIAN_POINT('Ctrl Pts',(-0.142550993842162,-0.00961078035088443,
1.50734168592779));
#16654=CARTESIAN_POINT('Ctrl Pts',(-0.142847161918882,-0.00687492249914849,
1.50724404681617));
#16655=CARTESIAN_POINT('Ctrl Pts',(-0.143058332724879,-0.00413406598225375,
1.5071466105924));
#16656=CARTESIAN_POINT('Ctrl Pts',(-0.143182669649515,-0.00139134585336764,
1.50704933585643));
#16657=CARTESIAN_POINT('Ctrl Pts',(-0.143203595382121,-0.00092974984559876,
1.50703296465278));
#16658=CARTESIAN_POINT('Ctrl Pts',(-0.143222061023464,-0.000468100854706259,
1.50701659802318));
#16659=CARTESIAN_POINT('Ctrl Pts',(-0.143238079070951,-6.41379011939899E-6,
1.50700023577028));
#16660=CARTESIAN_POINT('',(-0.00156744678985144,0.146109855568756,1.50365));
#16661=CARTESIAN_POINT('Ctrl Pts',(-0.00156962371672063,0.146072546381438,
1.50365));
#16662=CARTESIAN_POINT('Ctrl Pts',(-0.011711474284147,0.144648739717271,
1.50495065132295));
#16663=CARTESIAN_POINT('Ctrl Pts',(-0.0216501921041044,0.142222471223284,
1.50626105010813));
#16664=CARTESIAN_POINT('Ctrl Pts',(-0.0312062965385204,0.138804788898175,
1.50759029209282));
#16665=CARTESIAN_POINT('Ctrl Pts',(-0.0379863325344082,0.136379950477271,
1.50853338648503));
#16666=CARTESIAN_POINT('Ctrl Pts',(-0.0445735484268955,0.133455002060128,
1.5094859663039));
#16667=CARTESIAN_POINT('Ctrl Pts',(-0.0508923708069948,0.130021662144985,
1.51045128011208));
#16668=CARTESIAN_POINT('Ctrl Pts',(-0.053607485163773,0.128546401418451,
1.51086606268101));
#16669=CARTESIAN_POINT('Ctrl Pts',(-0.0562647183424556,0.126981576978965,
1.51128195276517));
#16670=CARTESIAN_POINT('Ctrl Pts',(-0.0588579379029418,0.125328026221608,
1.51169910067666));
#16671=CARTESIAN_POINT('Ctrl Pts',(-0.0624505046767585,0.123037247762191,
1.51227700458785));
#16672=CARTESIAN_POINT('Ctrl Pts',(-0.0659209207101175,0.120575889029892,
1.51285741907924));
#16673=CARTESIAN_POINT('Ctrl Pts',(-0.0692542752175272,0.117943487410649,
1.51344114883776));
#16674=CARTESIAN_POINT('Ctrl Pts',(-0.0735613784355843,0.114542101371374,
1.51419539934302));
#16675=CARTESIAN_POINT('Ctrl Pts',(-0.0776398170223455,0.110855132244726,
1.51495518495604));
#16676=CARTESIAN_POINT('Ctrl Pts',(-0.0814741368103916,0.106911749311875,
1.51572224163114));
#16677=CARTESIAN_POINT('Ctrl Pts',(-0.0845038784997064,0.103795829845314,
1.51632834224744));
#16678=CARTESIAN_POINT('Ctrl Pts',(-0.087381117690253,0.10051973853988,
1.51693898261853));
#16679=CARTESIAN_POINT('Ctrl Pts',(-0.0900959757046659,0.0970973798321736,
1.51755501917095));
#16680=CARTESIAN_POINT('Ctrl Pts',(-0.0920052356275281,0.0946905606587243,
1.51798825505079));
#16681=CARTESIAN_POINT('Ctrl Pts',(-0.093830595110286,0.092215607777745,
1.51842338946406));
#16682=CARTESIAN_POINT('Ctrl Pts',(-0.0955653742165971,0.0896840982544811,
1.51885969689116));
#16683=CARTESIAN_POINT('Ctrl Pts',(-0.0997851775729162,0.0835262696618028,
1.51992100293214));
#16684=CARTESIAN_POINT('Ctrl Pts',(-0.103479134251024,0.0770231540939269,
1.52099120961793));
#16685=CARTESIAN_POINT('Ctrl Pts',(-0.106606394578922,0.0702509006766953,
1.52207541818308));
#16686=CARTESIAN_POINT('Ctrl Pts',(-0.108879606303698,0.0653281362576702,
1.52286353153598));
#16687=CARTESIAN_POINT('Ctrl Pts',(-0.110852991156964,0.0602629640702717,
1.52365904329275));
#16688=CARTESIAN_POINT('Ctrl Pts',(-0.112503888351057,0.0550849881514033,
1.524463912762));
#16689=CARTESIAN_POINT('Ctrl Pts',(-0.113450017754745,0.0521174894567802,
1.52492518356294));
#16690=CARTESIAN_POINT('Ctrl Pts',(-0.114289979676541,0.0491121240008169,
1.52538965304266));
#16691=CARTESIAN_POINT('Ctrl Pts',(-0.115015874151616,0.0460903162170444,
1.52585530945224));
#16692=CARTESIAN_POINT('Ctrl Pts',(-0.117053612444637,0.0376074669234184,
1.52716250482259));
#16693=CARTESIAN_POINT('Ctrl Pts',(-0.118206139871793,0.0289652499882669,
1.52848357355921));
#16694=CARTESIAN_POINT('Ctrl Pts',(-0.11838625730212,0.0202925750432425,
1.52982832573377));
#16695=CARTESIAN_POINT('Ctrl Pts',(-0.118492077855379,0.015197303257165,
1.53061837930521));
#16696=CARTESIAN_POINT('Ctrl Pts',(-0.118261361656021,0.0100916471271278,
1.53141660760476));
#16697=CARTESIAN_POINT('Ctrl Pts',(-0.11766859746431,0.00500517689818842,
1.532225));
#16698=CARTESIAN_POINT('',(-0.115079981391543,0.0902137050004572,1.50365));
#16699=CARTESIAN_POINT('Origin',(0.,0.,1.50365));
#16700=CARTESIAN_POINT('Ctrl Pts',(-0.143238079070951,-6.41379011939899E-6,
1.50700023577028));
#16701=CARTESIAN_POINT('Ctrl Pts',(-0.143514357617001,0.00795674345750163,
1.50671802038504));
#16702=CARTESIAN_POINT('Ctrl Pts',(-0.14306421847979,0.0159310909218757,
1.50643710681857));
#16703=CARTESIAN_POINT('Ctrl Pts',(-0.141940608246003,0.023841490005315,
1.50615648267927));
#16704=CARTESIAN_POINT('Ctrl Pts',(-0.141317731836386,0.0282266413964,1.50600091791928));
#16705=CARTESIAN_POINT('Ctrl Pts',(-0.14048752132733,0.0325921818867556,
1.50584544210227));
#16706=CARTESIAN_POINT('Ctrl Pts',(-0.139456452513291,0.0369250818702156,
1.5056898827608));
#16707=CARTESIAN_POINT('Ctrl Pts',(-0.138790989895207,0.0397215809279161,
1.50558948313156));
#16708=CARTESIAN_POINT('Ctrl Pts',(-0.138042009924554,0.0425029011667524,
1.50548910366784));
#16709=CARTESIAN_POINT('Ctrl Pts',(-0.137214434473447,0.0452564915355094,
1.50538902890071));
#16710=CARTESIAN_POINT('Ctrl Pts',(-0.134176751889031,0.0553637675507716,
1.50502169637912));
#16711=CARTESIAN_POINT('Ctrl Pts',(-0.130076454936343,0.0651325632434767,
1.50465723703036));
#16712=CARTESIAN_POINT('Ctrl Pts',(-0.125018127980614,0.0743940890034878,
1.50429344851366));
#16713=CARTESIAN_POINT('Ctrl Pts',(-0.122034683484208,0.0798566160996726,
1.50407888293545));
#16714=CARTESIAN_POINT('Ctrl Pts',(-0.118716925567465,0.0851425936725427,
1.50386455072235));
#16715=CARTESIAN_POINT('Ctrl Pts',(-0.115078604842436,0.0902138214954005,
1.50365));
#16716=CARTESIAN_POINT('',(-0.05,-6.12323399573677E-18,1.6));
#16717=CARTESIAN_POINT('',(-0.1,-1.22464679914735E-17,1.55));
#16718=CARTESIAN_POINT('Origin',(0.,0.,1.6));
#16719=CARTESIAN_POINT('Ctrl Pts',(0.0850780204044575,-0.11908002747757,
-0.0164977839420936));
#16720=CARTESIAN_POINT('Ctrl Pts',(0.124677800165771,-0.0907875342533835,
-0.0138514540629917));
#16721=CARTESIAN_POINT('Ctrl Pts',(0.172751483861701,0.00791416360185712,
-0.00855879430478784));
#16722=CARTESIAN_POINT('Ctrl Pts',(0.0868617128612901,0.149726167188418,
-0.000619804667482127));
#16723=CARTESIAN_POINT('Ctrl Pts',(-0.078614020905812,0.154028602276276,
0.00731918496982359));
#16724=CARTESIAN_POINT('Ctrl Pts',(-0.172087192378165,0.0175525219725009,
0.0152581746071293));
#16725=CARTESIAN_POINT('Ctrl Pts',(-0.108045720411827,-0.135108484733225,
0.0231971642444351));
#16726=CARTESIAN_POINT('Ctrl Pts',(0.0549144151285058,-0.164025561655164,
0.0311361538817407));
#16727=CARTESIAN_POINT('Ctrl Pts',(0.167598788591005,-0.0428207868793744,
0.0390751435190465));
#16728=CARTESIAN_POINT('Ctrl Pts',(0.126860790413016,0.117600499296196,
0.0470141331563521));
#16729=CARTESIAN_POINT('Ctrl Pts',(-0.0300110592737492,0.170357625684536,
0.054953122793658));
#16730=CARTESIAN_POINT('Ctrl Pts',(-0.159409054995301,0.0671687418111174,
0.0628921124309635));
#16731=CARTESIAN_POINT('Ctrl Pts',(-0.142879399887002,-0.0975110083167992,
0.0708311020682695));
#16732=CARTESIAN_POINT('Ctrl Pts',(0.00444677171871267,-0.172924803493063,
0.078770091705575));
#16733=CARTESIAN_POINT('Ctrl Pts',(0.147702113712341,-0.0900384822365835,
0.0867090813428809));
#16734=CARTESIAN_POINT('Ctrl Pts',(0.155746353789385,0.0752722621313087,
0.0946480709801864));
#16735=CARTESIAN_POINT('Ctrl Pts',(0.021215449100004,0.17167621786987,0.102587060617492));
#16736=CARTESIAN_POINT('Ctrl Pts',(-0.132736728465598,0.110922462699857,
0.110526050254798));
#16737=CARTESIAN_POINT('Ctrl Pts',(-0.165177537004225,-0.0513732581591355,
0.118465039892104));
#16738=CARTESIAN_POINT('Ctrl Pts',(-0.0464096261145344,-0.166640254043574,
0.126404029529409));
#16739=CARTESIAN_POINT('Ctrl Pts',(0.114843114370719,-0.129359532685675,
0.134343019166715));
#16740=CARTESIAN_POINT('Ctrl Pts',(0.170964855654229,0.0263409830179588,
0.142282008804021));
#16741=CARTESIAN_POINT('Ctrl Pts',(0.0705799878925336,0.157928129946847,
0.150220998441327));
#16742=CARTESIAN_POINT('Ctrl Pts',(-0.0944160212638482,0.144942899583874,
0.158159988078632));
#16743=CARTESIAN_POINT('Ctrl Pts',(-0.172980633894512,-0.000727622896455919,
0.166098977715938));
#16744=CARTESIAN_POINT('Ctrl Pts',(-0.0931933312323777,-0.145732055885043,
0.174037967353244));
#16745=CARTESIAN_POINT('Ctrl Pts',(0.0719060791645076,-0.157328779695546,
0.181976956990549));
#16746=CARTESIAN_POINT('Ctrl Pts',(0.171180402159323,-0.0249017879745179,
0.189915946627855));
#16747=CARTESIAN_POINT('Ctrl Pts',(0.113750798721884,0.13032108391891,0.197854936265161));
#16748=CARTESIAN_POINT('Ctrl Pts',(-0.0478098650864174,0.16624393501773,
0.205793925902467));
#16749=CARTESIAN_POINT('Ctrl Pts',(-0.16560387403618,0.0499818570245514,
0.213732915539772));
#16750=CARTESIAN_POINT('Ctrl Pts',(-0.131798885878402,-0.112035185581475,
0.221671905177078));
#16751=CARTESIAN_POINT('Ctrl Pts',(0.0226589495323734,-0.171491694067101,
0.229610894814384));
#16752=CARTESIAN_POINT('Ctrl Pts',(0.156374069566079,-0.073959309724122,
0.237549884451689));
#16753=CARTESIAN_POINT('Ctrl Pts',(0.146939445926624,0.0912777539068999,
0.245488874088995));
#16754=CARTESIAN_POINT('Ctrl Pts',(0.00299182995941577,0.172956289510158,
0.253427863726301));
#16755=CARTESIAN_POINT('Ctrl Pts',(-0.143694601292225,0.0963051955349955,
0.261366853363607));
#16756=CARTESIAN_POINT('Ctrl Pts',(-0.15883847309497,-0.0685067047260848,
0.269305843000912));
#16757=CARTESIAN_POINT('Ctrl Pts',(-0.0285766086907934,-0.170605411881679,
0.277244832638218));
#16758=CARTESIAN_POINT('Ctrl Pts',(0.12784518248692,-0.116526556812001,
0.285183822275524));
#16759=CARTESIAN_POINT('Ctrl Pts',(0.167233470900423,0.0442243749325307,
0.293122811912829));
#16760=CARTESIAN_POINT('Ctrl Pts',(0.0535309779628647,0.164490922320707,
0.301061801550136));
#16761=CARTESIAN_POINT('Ctrl Pts',(-0.109175456582181,0.134177303623408,
0.309000791187441));
#16762=CARTESIAN_POINT('Ctrl Pts',(-0.171939242908932,-0.0189664407699395,
0.316939780824747));
#16763=CARTESIAN_POINT('Ctrl Pts',(-0.0773044361184472,-0.154747708493488,
0.324878770462053));
#16764=CARTESIAN_POINT('Ctrl Pts',(0.0880972839194656,-0.148868054644337,
0.332817760099358));
#16765=CARTESIAN_POINT('Ctrl Pts',(0.172851978230285,-0.00670989936239309,
0.340756749736664));
#16766=CARTESIAN_POINT('Ctrl Pts',(0.0993725327910066,0.141590708926387,
0.34869573937397));
#16767=CARTESIAN_POINT('Ctrl Pts',(-0.0650756559739905,0.160274727038081,
0.356634729011275));
#16768=CARTESIAN_POINT('Ctrl Pts',(-0.169951541620772,0.0322382168908211,
0.364573718648582));
#16769=CARTESIAN_POINT('Ctrl Pts',(-0.119248438453561,-0.125310171390688,
0.372512708285886));
#16770=CARTESIAN_POINT('Ctrl Pts',(0.0406184374886585,-0.168145685830938,
0.380451697923193));
#16771=CARTESIAN_POINT('Ctrl Pts',(0.163301917673335,-0.0570553486694088,
0.388390687560498));
#16772=CARTESIAN_POINT('Ctrl Pts',(0.136493684039406,0.106265249940549,
0.396329677197804));
#16773=CARTESIAN_POINT('Ctrl Pts',(-0.0152651628095069,0.172307295063139,
0.404268666835109));
#16774=CARTESIAN_POINT('Ctrl Pts',(-0.153049799296248,0.0806138205455782,
0.412207656472416));
#16775=CARTESIAN_POINT('Ctrl Pts',(-0.150727833715048,-0.0848760818555219,
0.420146646109721));
#16776=CARTESIAN_POINT('Ctrl Pts',(-0.0104248664208018,-0.172667748255674,
0.428085635747027));
#16777=CARTESIAN_POINT('Ctrl Pts',(0.139421351618932,-0.10239392482138,
0.436024625384332));
#16778=CARTESIAN_POINT('Ctrl Pts',(0.16163687742079,0.0616145192729195,
0.443963615021638));
#16779=CARTESIAN_POINT('Ctrl Pts',(0.0358849196425865,0.169219093691645,
0.451902604658944));
#16780=CARTESIAN_POINT('Ctrl Pts',(-0.122717222714247,0.121915185177559,
0.45984159429625));
#16781=CARTESIAN_POINT('Ctrl Pts',(-0.168980158036723,-0.0369937199732681,
0.467780583933555));
#16782=CARTESIAN_POINT('Ctrl Pts',(-0.0605533396431397,-0.162037409833775,
0.475719573570861));
#16783=CARTESIAN_POINT('Ctrl Pts',(0.103305911202344,-0.138746956140414,
0.483658563208167));
#16784=CARTESIAN_POINT('Ctrl Pts',(0.172595680358559,0.0115568269495825,
0.491597552845473));
#16785=CARTESIAN_POINT('Ctrl Pts',(0.0838859329010004,0.151281127008313,
0.499536542482778));
#16786=CARTESIAN_POINT('Ctrl Pts',(-0.0816156370489812,0.152517923263679,
0.507475532120084));
#16787=CARTESIAN_POINT('Ctrl Pts',(-0.172403684765527,0.0141350135070757,
0.51541452175739));
#16788=CARTESIAN_POINT('Ctrl Pts',(-0.105367974675403,-0.137187532379513,
0.523353511394695));
#16789=CARTESIAN_POINT('Ctrl Pts',(0.0581248948911363,-0.162924294448283,
0.531292501032001));
#16790=CARTESIAN_POINT('Ctrl Pts',(0.168408406744046,-0.039515030880773,
0.539231490669306));
#16791=CARTESIAN_POINT('Ctrl Pts',(0.124525564004667,0.120067535316156,
0.547170480306613));
#16792=CARTESIAN_POINT('Ctrl Pts',(-0.0333518982867267,0.169736501696743,
0.555109469943918));
#16793=CARTESIAN_POINT('Ctrl Pts',(-0.160697983451488,0.0640233335761385,
0.563048459581225));
#16794=CARTESIAN_POINT('Ctrl Pts',(-0.14093607811848,-0.100298808627811,
0.570987449218529));
#16795=CARTESIAN_POINT('Ctrl Pts',(0.00784314775175556,-0.172804265459278,
0.578926438855836));
#16796=CARTESIAN_POINT('Ctrl Pts',(0.149442509381278,-0.0871192603125336,
0.586865428493141));
#16797=CARTESIAN_POINT('Ctrl Pts',(0.154237495636292,0.0783174569774929,
0.594804418130446));
#16798=CARTESIAN_POINT('Ctrl Pts',(0.0178386252221998,0.172059909850489,
0.602743407767753));
#16799=CARTESIAN_POINT('Ctrl Pts',(-0.134890284021987,0.108293307291099,
0.610682397405058));
#16800=CARTESIAN_POINT('Ctrl Pts',(-0.164136382878957,-0.0546083962682395,
0.618621387042364));
#16801=CARTESIAN_POINT('Ctrl Pts',(-0.0431268722112106,-0.167519855601819,
0.62656037667967));
#16802=CARTESIAN_POINT('Ctrl Pts',(0.117362334288317,-0.127078368017432,
0.634499366316975));
#16803=CARTESIAN_POINT('Ctrl Pts',(0.170414367112955,0.0296946562375699,
0.642438355954282));
#16804=CARTESIAN_POINT('Ctrl Pts',(0.0674637261050104,0.159284257814778,
0.650377345591586));
#16805=CARTESIAN_POINT('Ctrl Pts',(-0.0972453325609638,0.143060037825677,
0.658316335228894));
#16806=CARTESIAN_POINT('Ctrl Pts',(-0.172932953925271,-0.00412584224812367,
0.666255324866198));
#16807=CARTESIAN_POINT('Ctrl Pts',(-0.0903123078403481,-0.147534796506203,
0.674194314503505));
#16808=CARTESIAN_POINT('Ctrl Pts',(0.0749830665657334,-0.155885755782802,
0.68213330414081));
#16809=CARTESIAN_POINT('Ctrl Pts',(0.17163658245605,-0.021533989188811,
0.690072293778116));
#16810=CARTESIAN_POINT('Ctrl Pts',(0.11116857013107,0.132530668686874,0.698011283415421));
#16811=CARTESIAN_POINT('Ctrl Pts',(-0.0510666492692211,0.165272582299639,
0.705950273052727));
#16812=CARTESIAN_POINT('Ctrl Pts',(-0.166553851089581,0.0467187736868841,
0.713889262690032));
#16813=CARTESIAN_POINT('Ctrl Pts',(-0.129572416918314,-0.114602870389546,
0.721828252327339));
#16814=CARTESIAN_POINT('Ctrl Pts',(0.0260236847639906,-0.171013440871999,
0.729767241964644));
#16815=CARTESIAN_POINT('Ctrl Pts',(0.157796886564457,-0.0708729265526718,
0.73770623160195));
#16816=CARTESIAN_POINT('Ctrl Pts',(0.145117853242075,0.0941468947867542,
0.745645221239255));
#16817=CARTESIAN_POINT('Ctrl Pts',(-0.000406629147419015,0.172981686256994,
0.753584210876562));
#16818=CARTESIAN_POINT('Ctrl Pts',(-0.145558870420566,0.0934635991681543,
0.761523200513868));
#16819=CARTESIAN_POINT('Ctrl Pts',(-0.157461941624574,-0.0716140074803496,
0.769462190151172));
#16820=CARTESIAN_POINT('Ctrl Pts',(-0.0252193968429213,-0.17113389830906,
0.777401179788479));
#16821=CARTESIAN_POINT('Ctrl Pts',(0.130109777350283,-0.113992433807847,
0.785340169425784));
#16822=CARTESIAN_POINT('Ctrl Pts',(0.166332367384696,0.0475012914327479,
0.793279159063091));
#16823=CARTESIAN_POINT('Ctrl Pts',(0.0502890745800368,0.165510839842773,
0.801218148700395));
#16824=CARTESIAN_POINT('Ctrl Pts',(-0.111790419467279,0.132006557575396,
0.809157138337702));
#16825=CARTESIAN_POINT('Ctrl Pts',(-0.171533445990104,-0.0223406811520247,
0.817096127975007));
#16826=CARTESIAN_POINT('Ctrl Pts',(-0.0742493586638003,-0.156236557391639,
0.825035117612313));
#16827=CARTESIAN_POINT('Ctrl Pts',(0.0910049278783345,-0.147108572929777,
0.832974107249618));
#16828=CARTESIAN_POINT('Ctrl Pts',(0.172950439922886,-0.00331277195964383,
0.840913096886925));
#16829=CARTESIAN_POINT('Ctrl Pts',(0.0965716772857839,0.143515644700454,
0.848852086524229));
#16830=CARTESIAN_POINT('Ctrl Pts',(-0.0682118374171683,0.158965324406771,
0.856791076161536));
#16831=CARTESIAN_POINT('Ctrl Pts',(-0.170552089827228,0.0288931442238776,
0.864730065798841));
#16832=CARTESIAN_POINT('Ctrl Pts',(-0.116763592698541,-0.127628729319482,
0.872669055436147));
#16833=CARTESIAN_POINT('Ctrl Pts',(0.0439139712140358,-0.167315248138923,
0.880608045073453));
#16834=CARTESIAN_POINT('Ctrl Pts',(0.164391304101163,-0.0538361241500125,
0.888547034710759));
#16835=CARTESIAN_POINT('Ctrl Pts',(0.134379664555536,0.108926281867684,
0.896486024348063));
#16836=CARTESIAN_POINT('Ctrl Pts',(-0.018647348250808,0.17197414204115,
0.904425013985371));
#16837=CARTESIAN_POINT('Ctrl Pts',(-0.154603991719776,0.0775914613336281,
0.912364003622676));
#16838=CARTESIAN_POINT('Ctrl Pts',(-0.149031276472826,-0.0878208845346985,
0.920302993259982));
#16839=CARTESIAN_POINT('Ctrl Pts',(-0.00703064139541984,-0.172839229369798,
0.928241982897287));
#16840=CARTESIAN_POINT('Ctrl Pts',(0.141406064038169,-0.099635105162837,
0.936180972534593));
#16841=CARTESIAN_POINT('Ctrl Pts',(0.160395209035295,0.064778129380991,
0.944119962171899));
#16842=CARTESIAN_POINT('Ctrl Pts',(0.03255353276219,0.169891426011666,0.952058951809204));
#16843=CARTESIAN_POINT('Ctrl Pts',(-0.125088671715395,0.119480765548496,
0.959997941446511));
#16844=CARTESIAN_POINT('Ctrl Pts',(-0.168220770124088,-0.040306347222682,
0.967936931083815));
#16845=CARTESIAN_POINT('Ctrl Pts',(-0.0573582824064844,-0.163195761485875,
0.975875920721122));
#16846=CARTESIAN_POINT('Ctrl Pts',(0.106011781834435,-0.136690640644722,
0.983814910358427));
#16847=CARTESIAN_POINT('Ctrl Pts',(0.17233532526783,0.014945393685262,0.991753899995733));
#16848=CARTESIAN_POINT('Ctrl Pts',(0.0808976893297158,0.152899944371113,
0.999692889633039));
#16849=CARTESIAN_POINT('Ctrl Pts',(-0.0845962369090198,0.150885074902754,
1.00763187927034));
#16850=CARTESIAN_POINT('Ctrl Pts',(-0.172648106016301,0.0107452601904448,
1.01557086890765));
#16851=CARTESIAN_POINT('Ctrl Pts',(-0.102652466413112,-0.13923110380544,
1.02350985854496));
#16852=CARTESIAN_POINT('Ctrl Pts',(0.0613144709582997,-0.161750934398167,
1.03144884818226));
#16853=CARTESIAN_POINT('Ctrl Pts',(0.169152212322519,-0.0361988700648799,
1.03938783781957));
#16854=CARTESIAN_POINT('Ctrl Pts',(0.122142696063681,0.12249077894222,1.04732682745687));
#16855=CARTESIAN_POINT('Ctrl Pts',(-0.0366800874558037,0.169048514669047,
1.05526581709418));
#16856=CARTESIAN_POINT('Ctrl Pts',(-0.161924764760067,0.0608539208677085,
1.06320480673148));
#16857=CARTESIAN_POINT('Ctrl Pts',(-0.138938417355371,-0.103048266896446,
1.07114379636879));
#16858=CARTESIAN_POINT('Ctrl Pts',(0.011236529066559,-0.172616828675865,
1.0790827860061));
#16859=CARTESIAN_POINT('Ctrl Pts',(0.151125203217684,-0.0841665140064042,
1.0870217756434));
#16860=CARTESIAN_POINT('Ctrl Pts',(0.152669111109608,0.0813324759279986,
1.09496076528071));
#16861=CARTESIAN_POINT('Ctrl Pts',(0.0144549108781955,0.172377158228925,
1.10289975491801));
#16862=CARTESIAN_POINT('Ctrl Pts',(-0.136991769602464,0.10562236594946,
1.11083874455532));
#16863=CARTESIAN_POINT('Ctrl Pts',(-0.163031873671196,-0.0578224635832477,
1.11877773419263));
#16864=CARTESIAN_POINT('Ctrl Pts',(-0.0398274706979539,-0.168334790537727,
1.12671672382993));
#16865=CARTESIAN_POINT('Ctrl Pts',(0.119836252144435,-0.124748153491552,
1.13465571346724));
#16866=CARTESIAN_POINT('Ctrl Pts',(0.169798099063322,0.0330368685268242,
1.14259470310454));
#16867=CARTESIAN_POINT('Ctrl Pts',(0.0643214233134591,0.160578901573361,
1.15053369274185));
#16868=CARTESIAN_POINT('Ctrl Pts',(-0.100037107244844,0.141121955420339,
1.15847268237915));
#16869=CARTESIAN_POINT('Ctrl Pts',(-0.172818522111203,-0.00752246920075927,
1.16641167201646));
#16870=CARTESIAN_POINT('Ctrl Pts',(-0.0873964240115842,-0.149280588817046,
1.17435066165376));
#16871=CARTESIAN_POINT('Ctrl Pts',(0.0780311106025284,-0.154382560238235,
1.18228965129107));
#16872=CARTESIAN_POINT('Ctrl Pts',(0.172026511281289,-0.01815787828917,
1.19022864092837));
#16873=CARTESIAN_POINT('Ctrl Pts',(0.10854343062882,0.134689096792963,1.19816763056568));
#16874=CARTESIAN_POINT('Ctrl Pts',(-0.0543037217972188,0.164237434607784,
1.20610662020299));
#16875=CARTESIAN_POINT('Ctrl Pts',(-0.167439538594998,0.0434376569656869,
1.21404560984029));
#16876=CARTESIAN_POINT('Ctrl Pts',(-0.127295933190098,-0.117126318651471,
1.2219845994776));
#16877=CARTESIAN_POINT('Ctrl Pts',(0.0293783748903316,-0.170469176734012,
1.2299235891149));
#16878=CARTESIAN_POINT('Ctrl Pts',(0.159158794190081,-0.0677591865323411,
1.23786257875221));
#16879=CARTESIAN_POINT('Ctrl Pts',(0.143240245273553,0.0969796950995427,
1.24580156838952));
#16880=CARTESIAN_POINT('Ctrl Pts',(-0.00380493129617075,0.172940312320012,
1.25374055802682));
#16881=CARTESIAN_POINT('Ctrl Pts',(-0.147366954032488,0.0905859259858403,
1.26167954766413));
#16882=CARTESIAN_POINT('Ctrl Pts',(-0.156024630070406,-0.074693667330688,
1.26961853730143));
#16883=CARTESIAN_POINT('Ctrl Pts',(-0.0218524503424686,-0.171596327294885,
1.27755752693874));
#16884=CARTESIAN_POINT('Ctrl Pts',(0.132324150022753,-0.111414309889572,
1.28549651657604));
#16885=CARTESIAN_POINT('Ctrl Pts',(0.165367059817933,0.0507598725070622,
1.29343550621335));
#16886=CARTESIAN_POINT('Ctrl Pts',(0.0470277596764783,0.166466870408131,
1.30137449585065));
#16887=CARTESIAN_POINT('Ctrl Pts',(-0.114362231391601,0.129784857201791,
1.30931348548797));
#16888=CARTESIAN_POINT('Ctrl Pts',(-0.171061437441431,-0.0257062980954763,
1.31725247512526));
#16889=CARTESIAN_POINT('Ctrl Pts',(-0.071165620995849,-0.157665099140374,
1.32519146476257));
#16890=CARTESIAN_POINT('Ctrl Pts',(0.0938774439379855,-0.145292307632914,
1.33313045439988));
#16891=CARTESIAN_POINT('Ctrl Pts',(0.172982143233999,8.56343898915854E-5,
1.34106944403719));
#16892=CARTESIAN_POINT('Ctrl Pts',(0.0937335447930804,0.145385183220099,
1.34900843367449));
#16893=CARTESIAN_POINT('Ctrl Pts',(-0.0713216883190155,0.157594562185848,
1.3569474233118));
#16894=CARTESIAN_POINT('Ctrl Pts',(-0.171086806821499,0.0255369173285507,
1.3648864129491));
#16895=CARTESIAN_POINT('Ctrl Pts',(-0.114233673229396,-0.129898019862958,
1.37282540258641));
#16896=CARTESIAN_POINT('Ctrl Pts',(0.0471925482590101,-0.166420232464351,
1.38076439222371));
#16897=CARTESIAN_POINT('Ctrl Pts',(0.165417247017141,-0.0505961085897048,
1.38870338186102));
#16898=CARTESIAN_POINT('Ctrl Pts',(0.132213753266125,0.111545248710567,
1.39664237149832));
#16899=CARTESIAN_POINT('Ctrl Pts',(-0.0220222951247444,0.17157464463752,
1.40458136113563));
#16900=CARTESIAN_POINT('Ctrl Pts',(-0.156098584526576,0.0745390809398717,
1.41252035077293));
#16901=CARTESIAN_POINT('Ctrl Pts',(-0.147277046608992,-0.0907316537045687,
1.42045934041024));
#16902=CARTESIAN_POINT('Ctrl Pts',(-0.00363398118293899,-0.172944250658386,
1.42839833004755));
#16903=CARTESIAN_POINT('Ctrl Pts',(0.143336722904634,-0.0968373407211472,
1.43633731968485));
#16904=CARTESIAN_POINT('Ctrl Pts',(0.159090624036536,0.0679158129692223,
1.44427630932216));
#16905=CARTESIAN_POINT('Ctrl Pts',(0.0292114869387437,0.170499931406899,
1.45221529895946));
#16906=CARTESIAN_POINT('Ctrl Pts',(-0.127415456569397,0.116996902323752,
1.46015428859677));
#16907=CARTESIAN_POINT('Ctrl Pts',(-0.167389576437263,-0.0435971050111283,
1.46809327823408));
#16908=CARTESIAN_POINT('Ctrl Pts',(-0.0541541359620402,-0.164303103757731,
1.47603226787138));
#16909=CARTESIAN_POINT('Ctrl Pts',(0.108701533888403,-0.13455879509903,
1.48397125750869));
#16910=CARTESIAN_POINT('Ctrl Pts',(0.171961157005542,0.0182848320604298,
1.49191024714599));
#16911=CARTESIAN_POINT('Ctrl Pts',(0.0779697431325927,0.154543202561513,
1.4998492367833));
#16912=CARTESIAN_POINT('Ctrl Pts',(-0.0877325682749983,0.149025855561406,
1.5077882264206));
#16913=CARTESIAN_POINT('Ctrl Pts',(-0.144149484752264,0.0548439265155397,
1.51308088617881));
#16914=CARTESIAN_POINT('Ctrl Pts',(-0.146217781693078,0.00621955116994065,
1.51572721605791));
#16915=CARTESIAN_POINT('Ctrl Pts',(0.0795408277542855,-0.111329858282327,
-0.0109985226280624));
#16916=CARTESIAN_POINT('Ctrl Pts',(0.116563307192903,-0.0848787452970238,
-0.00835219274896048));
#16917=CARTESIAN_POINT('Ctrl Pts',(0.16150817751539,0.00739908052493189,
-0.00305953299075667));
#16918=CARTESIAN_POINT('Ctrl Pts',(0.0812084309002137,0.139981433724326,
0.00487945664654907));
#16919=CARTESIAN_POINT('Ctrl Pts',(-0.0734975292821143,0.144003850402812,
0.0128184462838548));
#16920=CARTESIAN_POINT('Ctrl Pts',(-0.160887120581772,0.0164101388376342,
0.0207574359211605));
#16921=CARTESIAN_POINT('Ctrl Pts',(-0.101013704785435,-0.126315124179183,
0.0286964255584662));
#16922=CARTESIAN_POINT('Ctrl Pts',(0.0513403816191153,-0.153350170642076,
0.0366354151957719));
#16923=CARTESIAN_POINT('Ctrl Pts',(0.156690838735662,-0.0400338514845966,
0.0445744048330777));
#16924=CARTESIAN_POINT('Ctrl Pts',(0.118604220350264,0.109946623274354,
0.0525133944703833));
#16925=CARTESIAN_POINT('Ctrl Pts',(-0.0280578283917351,0.15927012049393,
0.0604523841076892));
#16926=CARTESIAN_POINT('Ctrl Pts',(-0.14903412333264,0.0627971513379326,
0.0683913737449947));
#16927=CARTESIAN_POINT('Ctrl Pts',(-0.133580279395553,-0.0911646307683348,
0.0763303633823007));
#16928=CARTESIAN_POINT('Ctrl Pts',(0.0041573593468571,-0.161670216863261,
0.0842693530196062));
#16929=CARTESIAN_POINT('Ctrl Pts',(0.138089113144455,-0.0841784443595545,
0.0922083426569122));
#16930=CARTESIAN_POINT('Ctrl Pts',(0.14560980428584,0.0703732645446943,
0.100147332294218));
#16931=CARTESIAN_POINT('Ctrl Pts',(0.0198346691022095,0.160502893816501,
0.108086321931524));
#16932=CARTESIAN_POINT('Ctrl Pts',(-0.124097730593135,0.103703218031488,
0.116025311568829));
#16933=CARTESIAN_POINT('Ctrl Pts',(-0.154427171169137,-0.0480296962598115,
0.123964301206135));
#16934=CARTESIAN_POINT('Ctrl Pts',(-0.0433891157712434,-0.155794689166463,
0.13190329084344));
#16935=CARTESIAN_POINT('Ctrl Pts',(0.107368699171666,-0.12094033522185,
0.139842280480747));
#16936=CARTESIAN_POINT('Ctrl Pts',(0.15983782968835,0.0246266142906177,
0.147781270118052));
#16937=CARTESIAN_POINT('Ctrl Pts',(0.0659863808909888,0.147649582370873,
0.155720259755358));
#16938=CARTESIAN_POINT('Ctrl Pts',(-0.0882710769349216,0.135509478890084,
0.163659249392663));
#16939=CARTESIAN_POINT('Ctrl Pts',(-0.161722413615419,-0.00068026650363694,
0.171598239029969));
#16940=CARTESIAN_POINT('Ctrl Pts',(-0.0871279640988751,-0.136247273976568,
0.179537228667275));
#16941=CARTESIAN_POINT('Ctrl Pts',(0.0672261652318651,-0.147089240053593,
0.187476218304581));
#16942=CARTESIAN_POINT('Ctrl Pts',(0.160039347628626,-0.023281087390596,
0.195415207941886));
#16943=CARTESIAN_POINT('Ctrl Pts',(0.106347475470598,0.121839305139765,
0.203354197579192));
#16944=CARTESIAN_POINT('Ctrl Pts',(-0.0446982220051161,0.15542416405057,
0.211293187216498));
#16945=CARTESIAN_POINT('Ctrl Pts',(-0.154825760608133,0.0467288526640558,
0.219232176853804));
#16946=CARTESIAN_POINT('Ctrl Pts',(-0.12322092627477,-0.104743520787053,
0.227171166491109));
#16947=CARTESIAN_POINT('Ctrl Pts',(0.0211842211805034,-0.160330379506191,
0.235110156128415));
#16948=CARTESIAN_POINT('Ctrl Pts',(0.146196665995071,-0.0691457639426259,
0.24304914576572));
#16949=CARTESIAN_POINT('Ctrl Pts',(0.137376082602736,0.0853370596399817,
0.250988135403027));
#16950=CARTESIAN_POINT('Ctrl Pts',(0.00279711058556459,0.161699653653757,
0.258927125040332));
#16951=CARTESIAN_POINT('Ctrl Pts',(-0.134342424474264,0.0900372967480426,
0.266866114677638));
#16952=CARTESIAN_POINT('Ctrl Pts',(-0.148500677015507,-0.0640480346713102,
0.274805104314944));
#16953=CARTESIAN_POINT('Ctrl Pts',(-0.0267167371651392,-0.159501779847699,
0.282744093952249));
#16954=CARTESIAN_POINT('Ctrl Pts',(0.119524544542348,-0.108942576944327,
0.290683083589556));
#16955=CARTESIAN_POINT('Ctrl Pts',(0.156349297273321,0.0413460888291301,
0.29862207322686));
#16956=CARTESIAN_POINT('Ctrl Pts',(0.0500469836677093,0.153785243912065,
0.306561062864167));
#16957=CARTESIAN_POINT('Ctrl Pts',(-0.102069913541897,0.125444547784578,
0.314500052501472));
#16958=CARTESIAN_POINT('Ctrl Pts',(-0.160748800211922,-0.0177320345633525,
0.322439042138778));
#16959=CARTESIAN_POINT('Ctrl Pts',(-0.0722731771226978,-0.144676154524232,
0.330378031776084));
#16960=CARTESIAN_POINT('Ctrl Pts',(0.082363586418043,-0.139179170322594,
0.338317021413389));
#16961=CARTESIAN_POINT('Ctrl Pts',(0.16160213133829,-0.00627319426210969,
0.346256011050695));
#16962=CARTESIAN_POINT('Ctrl Pts',(0.0929050003357002,0.132375461215256,
0.354195000688001));
#16963=CARTESIAN_POINT('Ctrl Pts',(-0.0608402912787218,0.149843454232904,
0.362133990325306));
#16964=CARTESIAN_POINT('Ctrl Pts',(-0.158890465884947,0.0301400343429239,
0.370072979962613));
#16965=CARTESIAN_POINT('Ctrl Pts',(-0.1114873084483,-0.117154521356547,
0.378011969599918));
#16966=CARTESIAN_POINT('Ctrl Pts',(0.0379748391485164,-0.157202141877815,
0.385950959237223));
#16967=CARTESIAN_POINT('Ctrl Pts',(0.152673624090564,-0.0533419752763387,
0.39388994887453));
#16968=CARTESIAN_POINT('Ctrl Pts',(0.127610169584502,0.0993491139263089,
0.401828938511835));
#16969=CARTESIAN_POINT('Ctrl Pts',(-0.014271649480085,0.16109289816887,
0.409767928149142));
#16970=CARTESIAN_POINT('Ctrl Pts',(-0.143088751545671,0.0753671745551693,
0.417706917786446));
#16971=CARTESIAN_POINT('Ctrl Pts',(-0.140917908083783,-0.0793520321139836,
0.425645907423752));
#16972=CARTESIAN_POINT('Ctrl Pts',(-0.00974637750615997,-0.161429891732714,
0.433584897061058));
#16973=CARTESIAN_POINT('Ctrl Pts',(0.130347293715478,-0.0957297489831606,
0.441523886698364));
#16974=CARTESIAN_POINT('Ctrl Pts',(0.15111695082405,0.0576044181723055,
0.449462876335669));
#16975=CARTESIAN_POINT('Ctrl Pts',(0.0335493961742207,0.158205688379633,
0.457401865972975));
#16976=CARTESIAN_POINT('Ctrl Pts',(-0.114730331382826,0.113980493419335,
0.465340855610281));
#16977=CARTESIAN_POINT('Ctrl Pts',(-0.157982303542021,-0.03458603167299,
0.473279845247587));
#16978=CARTESIAN_POINT('Ctrl Pts',(-0.0566123040428622,-0.151491415104245,
0.481218834884892));
#16979=CARTESIAN_POINT('Ctrl Pts',(0.0965823799129518,-0.129716790392294,
0.489157824522198));
#16980=CARTESIAN_POINT('Ctrl Pts',(0.161362514281243,0.0108046658515635,
0.497096814159504));
#16981=CARTESIAN_POINT('Ctrl Pts',(0.0784263257203939,0.141435191000425,
0.50503580379681));
#16982=CARTESIAN_POINT('Ctrl Pts',(-0.076303789130349,0.14259149197508,
0.512974793434115));
#16983=CARTESIAN_POINT('Ctrl Pts',(-0.161183014472451,0.0132150544797126,
0.520913783071421));
#16984=CARTESIAN_POINT('Ctrl Pts',(-0.0985102366584373,-0.128258859705,
0.528852772708727));
#16985=CARTESIAN_POINT('Ctrl Pts',(0.0543419114689404,-0.152320577983508,
0.536791762346032));
#16986=CARTESIAN_POINT('Ctrl Pts',(0.157447763940923,-0.0369432463290883,
0.544730751983338));
#16987=CARTESIAN_POINT('Ctrl Pts',(0.116420979124965,0.112253095453589,
0.552669741620643));
#16988=CARTESIAN_POINT('Ctrl Pts',(-0.0311812332291155,0.158689421555565,
0.56060873125795));
#16989=CARTESIAN_POINT('Ctrl Pts',(-0.150239163551416,0.0598564579197502,
0.568547720895255));
#16990=CARTESIAN_POINT('Ctrl Pts',(-0.131763436204723,-0.0937709907106254,
0.576486710532561));
#16991=CARTESIAN_POINT('Ctrl Pts',(0.00733268664935855,-0.161557523891122,
0.584425700169866));
#16992=CARTESIAN_POINT('Ctrl Pts',(0.139716237417787,-0.0814492162095161,
0.592364689807173));
#16993=CARTESIAN_POINT('Ctrl Pts',(0.144199148209332,0.0732202668325601,
0.600303679444478));
#16994=CARTESIAN_POINT('Ctrl Pts',(0.0166776214282734,0.160861613702037,
0.608242669081784));
#16995=CARTESIAN_POINT('Ctrl Pts',(-0.126111124778327,0.101245177793678,
0.616181658719089));
#16996=CARTESIAN_POINT('Ctrl Pts',(-0.153453779210204,-0.0510542795996006,
0.624120648356396));
#16997=CARTESIAN_POINT('Ctrl Pts',(-0.0403200156494649,-0.156617042997737,
0.6320596379937));
#16998=CARTESIAN_POINT('Ctrl Pts',(0.10972395892722,-0.118807637198397,
0.639998627631007));
#16999=CARTESIAN_POINT('Ctrl Pts',(0.159323168980049,0.0277620180369333,
0.647937617268312));
#17000=CARTESIAN_POINT('Ctrl Pts',(0.0630729369615192,0.148917448414806,
0.655876606905618));
#17001=CARTESIAN_POINT('Ctrl Pts',(-0.0909162461746061,0.133749160748195,
0.663815596542924));
#17002=CARTESIAN_POINT('Ctrl Pts',(-0.161677836835157,-0.00385731715476066,
0.671754586180229));
#17003=CARTESIAN_POINT('Ctrl Pts',(-0.0844344483789265,-0.137932685561743,
0.679693575817536));
#17004=CARTESIAN_POINT('Ctrl Pts',(0.0701028908975481,-0.145740133481257,
0.687632565454841));
#17005=CARTESIAN_POINT('Ctrl Pts',(0.1604658380222,-0.0201324774223393,
0.695571555092147));
#17006=CARTESIAN_POINT('Ctrl Pts',(0.10393330787963,0.123905081947942,0.703510544729453));
#17007=CARTESIAN_POINT('Ctrl Pts',(-0.0477430426119635,0.15451603056473,
0.711449534366758));
#17008=CARTESIAN_POINT('Ctrl Pts',(-0.155713909636705,0.0436781428746717,
0.719388524004064));
#17009=CARTESIAN_POINT('Ctrl Pts',(-0.121139364160222,-0.10714409115852,
0.72732751364137));
#17010=CARTESIAN_POINT('Ctrl Pts',(0.0243299669821161,-0.159883252800214,
0.735266503278675));
#17011=CARTESIAN_POINT('Ctrl Pts',(0.147526880793862,-0.0662602540182413,
0.743205492915981));
#17012=CARTESIAN_POINT('Ctrl Pts',(0.135673045916277,0.0880194662056535,
0.751144482553287));
#17013=CARTESIAN_POINT('Ctrl Pts',(-0.000380164216571841,0.161723397486253,
0.759083472190592));
#17014=CARTESIAN_POINT('Ctrl Pts',(-0.136085360063504,0.0873806419964673,
0.767022461827899));
#17015=CARTESIAN_POINT('Ctrl Pts',(-0.147213735311121,-0.0669531026545853,
0.774961451465203));
#17016=CARTESIAN_POINT('Ctrl Pts',(-0.023578025097595,-0.159995870421162,
0.78290044110251));
#17017=CARTESIAN_POINT('Ctrl Pts',(0.121641751185188,-0.106573384050283,
0.790839430739816));
#17018=CARTESIAN_POINT('Ctrl Pts',(0.155506840911589,0.0444097314676148,
0.798778420377121));
#17019=CARTESIAN_POINT('Ctrl Pts',(0.047016075363265,0.15473878142458,0.806717410014428));
#17020=CARTESIAN_POINT('Ctrl Pts',(-0.104514684958047,0.123415081928621,
0.814656399651731));
#17021=CARTESIAN_POINT('Ctrl Pts',(-0.16036941405942,-0.020886666885039,
0.82259538928904));
#17022=CARTESIAN_POINT('Ctrl Pts',(-0.0694169354231278,-0.146068103622213,
0.830534378926343));
#17023=CARTESIAN_POINT('Ctrl Pts',(0.085081990139753,-0.137534202194171,
0.838473368563651));
#17024=CARTESIAN_POINT('Ctrl Pts',(0.161694184779289,-0.00309716449182502,
0.846412358200955));
#17025=CARTESIAN_POINT('Ctrl Pts',(0.0902864348795877,0.134175115040242,
0.854351347838261));
#17026=CARTESIAN_POINT('Ctrl Pts',(-0.0637723584188847,0.148619272374149,
0.862290337475567));
#17027=CARTESIAN_POINT('Ctrl Pts',(-0.159451928190027,0.0270126713934565,
0.870229327112872));
#17028=CARTESIAN_POINT('Ctrl Pts',(-0.109164185657521,-0.119322178948671,
0.878168316750179));
#17029=CARTESIAN_POINT('Ctrl Pts',(0.0410558873341998,-0.156425752146281,
0.886107306387484));
#17030=CARTESIAN_POINT('Ctrl Pts',(0.153692109215179,-0.0503322698109037,
0.894046296024789));
#17031=CARTESIAN_POINT('Ctrl Pts',(0.125633738317809,0.101836956040625,
0.901985285662096));
#17032=CARTESIAN_POINT('Ctrl Pts',(-0.0174337097671096,0.160781427979367,
0.909924275299401));
#17033=CARTESIAN_POINT('Ctrl Pts',(-0.144541791370401,0.072541521673891,
0.917863264936708));
#17034=CARTESIAN_POINT('Ctrl Pts',(-0.13933176907,-0.082105176128868,0.925802254574012));
#17035=CARTESIAN_POINT('Ctrl Pts',(-0.00657306121577474,-0.161590212220858,
0.933741244211319));
#17036=CARTESIAN_POINT('Ctrl Pts',(0.132202833700187,-0.0931504835251481,
0.941680233848624));
#17037=CARTESIAN_POINT('Ctrl Pts',(0.149956094815541,0.0605621288182698,
0.949619223485929));
#17038=CARTESIAN_POINT('Ctrl Pts',(0.0304348282896272,0.158834262822317,
0.957558213123236));
#17039=CARTESIAN_POINT('Ctrl Pts',(-0.116947437700435,0.111704514835484,
0.965497202760542));
#17040=CARTESIAN_POINT('Ctrl Pts',(-0.157272339407096,-0.0376830608728604,
0.973436192397847));
#17041=CARTESIAN_POINT('Ctrl Pts',(-0.0536251929639052,-0.152574376940928,
0.981375182035153));
#17042=CARTESIAN_POINT('Ctrl Pts',(0.0991121424632477,-0.127794307524525,
0.989314171672459));
#17043=CARTESIAN_POINT('Ctrl Pts',(0.161119104064031,0.0139726921146952,
0.997253161309763));
#17044=CARTESIAN_POINT('Ctrl Pts',(0.0756325681075411,0.142948649734045,
1.00519215094707));
#17045=CARTESIAN_POINT('Ctrl Pts',(-0.0790904005129918,0.141064915432658,
1.01313114058437));
#17046=CARTESIAN_POINT('Ctrl Pts',(-0.161411527883023,0.0100459188627121,
1.02107013022168));
#17047=CARTESIAN_POINT('Ctrl Pts',(-0.095971463730607,-0.130169427934261,
1.02900911985899));
#17048=CARTESIAN_POINT('Ctrl Pts',(0.0573238981132153,-0.151223584550935,
1.03694810949629));
#17049=CARTESIAN_POINT('Ctrl Pts',(0.158143159897702,-0.0338429135403315,
1.0448870991336));
#17050=CARTESIAN_POINT('Ctrl Pts',(0.114193197054413,0.114518625410106,
1.0528260887709));
#17051=CARTESIAN_POINT('Ctrl Pts',(-0.0342928115212847,0.158046211271557,
1.06076507840821));
#17052=CARTESIAN_POINT('Ctrl Pts',(-0.151386101389109,0.0568933223281485,
1.06870406804552));
#17053=CARTESIAN_POINT('Ctrl Pts',(-0.129895790602315,-0.0963415040526547,
1.07664305768282));
#17054=CARTESIAN_POINT('Ctrl Pts',(0.0105052141409744,-0.161382286187737,
1.08458204732013));
#17055=CARTESIAN_POINT('Ctrl Pts',(0.141289415307547,-0.0786886455683398,
1.09252103695743));
#17056=CARTESIAN_POINT('Ctrl Pts',(0.14273283995608,0.076039057183793,1.10046002659474));
#17057=CARTESIAN_POINT('Ctrl Pts',(0.013514131745196,0.161158214381091,
1.10839901623204));
#17058=CARTESIAN_POINT('Ctrl Pts',(-0.128075837894479,0.0987480712062529,
1.11633800586935));
#17059=CARTESIAN_POINT('Ctrl Pts',(-0.152421155552179,-0.0540591635106084,
1.12427699550666));
#17060=CARTESIAN_POINT('Ctrl Pts',(-0.0372353514058616,-0.157378938949945,
1.13221598514396));
#17061=CARTESIAN_POINT('Ctrl Pts',(0.11203686504723,-0.116629081663695,
1.14015497478127));
#17062=CARTESIAN_POINT('Ctrl Pts',(0.158747009937404,0.0308867067726846,
1.14809396441857));
#17063=CARTESIAN_POINT('Ctrl Pts',(0.0601351468730053,0.150127831962932,
1.15603295405588));
#17064=CARTESIAN_POINT('Ctrl Pts',(-0.0935263218228598,0.13193721592339,
1.16397194369318));
#17065=CARTESIAN_POINT('Ctrl Pts',(-0.161570852667341,-0.00703287904607843,
1.17191093333049));
#17066=CARTESIAN_POINT('Ctrl Pts',(-0.0817083410685703,-0.13956485524354,
1.17984992296779));
#17067=CARTESIAN_POINT('Ctrl Pts',(0.0729525569401478,-0.144334771469742,
1.1877889126051));
#17068=CARTESIAN_POINT('Ctrl Pts',(0.160830388835411,-0.016976096323307,
1.19572790224241));
#17069=CARTESIAN_POINT('Ctrl Pts',(0.101479022178261,0.125923031559255,
1.20366689187971));
#17070=CARTESIAN_POINT('Ctrl Pts',(-0.0507694344715009,0.153548254118279,
1.21160588151702));
#17071=CARTESIAN_POINT('Ctrl Pts',(-0.15654195331917,0.0406105733811438,
1.21954487115432));
#17072=CARTESIAN_POINT('Ctrl Pts',(-0.119011042423884,-0.109503304062093,
1.22748386079163));
#17073=CARTESIAN_POINT('Ctrl Pts',(0.0274663214511058,-0.159374411387982,
1.23542285042894));
#17074=CARTESIAN_POINT('Ctrl Pts',(0.148800150427453,-0.0633491677300162,
1.24336184006624));
#17075=CARTESIAN_POINT('Ctrl Pts',(0.133917639627974,0.0906678973829495,
1.25130082970354));
#17076=CARTESIAN_POINT('Ctrl Pts',(-0.00355729227603857,0.161684716318317,
1.25923981934086));
#17077=CARTESIAN_POINT('Ctrl Pts',(-0.137775766897813,0.0846902584421788,
1.26717880897816));
#17078=CARTESIAN_POINT('Ctrl Pts',(-0.14586996931591,-0.0698323268364953,
1.27511779861547));
#17079=CARTESIAN_POINT('Ctrl Pts',(-0.0204302119447119,-0.160428202816007,
1.28305678825277));
#17080=CARTESIAN_POINT('Ctrl Pts',(0.123712004283314,-0.104163053984564,
1.29099577789008));
#17081=CARTESIAN_POINT('Ctrl Pts',(0.15460435913624,0.0474562320176185,
1.29893476752738));
#17082=CARTESIAN_POINT('Ctrl Pts',(0.043967018911749,0.155632589980133,
1.30687375716469));
#17083=CARTESIAN_POINT('Ctrl Pts',(-0.106919113837756,0.121337978043289,
1.31481274680199));
#17084=CARTESIAN_POINT('Ctrl Pts',(-0.159928125575155,-0.0240332370134145,
1.3227517364393));
#17085=CARTESIAN_POINT('Ctrl Pts',(-0.0665338988230771,-0.147403670583407,
1.33069072607661));
#17086=CARTESIAN_POINT('Ctrl Pts',(0.0877675522160205,-0.135836146169277,
1.33862971571391));
#17087=CARTESIAN_POINT('Ctrl Pts',(0.161723824721502,8.00609866524728E-5,
1.34656870535122));
#17088=CARTESIAN_POINT('Ctrl Pts',(0.0876330185603928,0.135922977069285,
1.35450769498852));
#17089=CARTESIAN_POINT('Ctrl Pts',(-0.0666798087068602,0.147337724435113,
1.36244668462583));
#17090=CARTESIAN_POINT('Ctrl Pts',(-0.159951843822013,0.0238748801740983,
1.37038567426313));
#17091=CARTESIAN_POINT('Ctrl Pts',(-0.106798922716859,-0.121443775659372,
1.37832466390044));
#17092=CARTESIAN_POINT('Ctrl Pts',(0.0441210824430389,-0.155588987406456,
1.38626365353774));
#17093=CARTESIAN_POINT('Ctrl Pts',(0.154651279966657,-0.0473031264624986,
1.39420264317505));
#17094=CARTESIAN_POINT('Ctrl Pts',(0.123608792556459,0.10428547082216,1.40214163281236));
#17095=CARTESIAN_POINT('Ctrl Pts',(-0.020589002599541,0.160407931346284,
1.41008062244966));
#17096=CARTESIAN_POINT('Ctrl Pts',(-0.145939110542184,0.0696878015005003,
1.41801961208697));
#17097=CARTESIAN_POINT('Ctrl Pts',(-0.137691710982408,-0.0848265016612731,
1.42595860172427));
#17098=CARTESIAN_POINT('Ctrl Pts',(-0.00339746822928561,-0.161688398335044,
1.43389759136158));
#17099=CARTESIAN_POINT('Ctrl Pts',(0.134007838137522,-0.0905348079547059,
1.44183658099889));
#17100=CARTESIAN_POINT('Ctrl Pts',(0.148736417039967,0.0634956003383226,
1.44977557063619));
#17101=CARTESIAN_POINT('Ctrl Pts',(0.0273102951854726,0.159403164432859,
1.4577145602735));
#17102=CARTESIAN_POINT('Ctrl Pts',(-0.119122786779006,0.109382310628272,
1.4656535499108));
#17103=CARTESIAN_POINT('Ctrl Pts',(-0.156495242883694,-0.0407596439572756,
1.47359253954811));
#17104=CARTESIAN_POINT('Ctrl Pts',(-0.0506295842364637,-0.153609649276743,
1.48153152918541));
#17105=CARTESIAN_POINT('Ctrl Pts',(0.10162683549218,-0.125801210382132,
1.48947051882272));
#17106=CARTESIAN_POINT('Ctrl Pts',(0.160769288057966,0.017094787472962,
1.49740950846002));
#17107=CARTESIAN_POINT('Ctrl Pts',(0.0728951834924312,0.144484958595688,
1.50534849809733));
#17108=CARTESIAN_POINT('Ctrl Pts',(-0.0820226078184241,0.139326700971572,
1.51328748773464));
#17109=CARTESIAN_POINT('Ctrl Pts',(-0.134767702434085,0.0512744806661359,
1.51858014749284));
#17110=CARTESIAN_POINT('Ctrl Pts',(-0.136701386950156,0.00581475974600206,
1.52122647737194));
#17111=CARTESIAN_POINT('Ctrl Pts',(0.0740036351041134,-0.103579689087085,
-0.0054992613140312));
#17112=CARTESIAN_POINT('Ctrl Pts',(0.108448814220036,-0.0789699563406641,
-0.00285293143492929));
#17113=CARTESIAN_POINT('Ctrl Pts',(0.150264871169078,0.00688399744800666,
0.00243972832327453));
#17114=CARTESIAN_POINT('Ctrl Pts',(0.0755551489391376,0.130236700260234,
0.0103787179605803));
#17115=CARTESIAN_POINT('Ctrl Pts',(-0.0683810376584167,0.133979098529349,
0.0183177075978859));
#17116=CARTESIAN_POINT('Ctrl Pts',(-0.14968704878538,0.0152677557027674,
0.0262566972351917));
#17117=CARTESIAN_POINT('Ctrl Pts',(-0.0939816891590436,-0.11752176362514,
0.0341956868724974));
#17118=CARTESIAN_POINT('Ctrl Pts',(0.0477663481097245,-0.142674779628989,
0.0421346765098031));
#17119=CARTESIAN_POINT('Ctrl Pts',(0.14578288888032,-0.0372469160898187,
0.0500736661471088));
#17120=CARTESIAN_POINT('Ctrl Pts',(0.110347650287512,0.102292747252513,
0.0580126557844146));
#17121=CARTESIAN_POINT('Ctrl Pts',(-0.0261045975097209,0.148182615303324,
0.0659516454217203));
#17122=CARTESIAN_POINT('Ctrl Pts',(-0.13865919166998,0.0584255608647477,
0.073890635059026));
#17123=CARTESIAN_POINT('Ctrl Pts',(-0.124281158904105,-0.0848182532198701,
0.0818296246963318));
#17124=CARTESIAN_POINT('Ctrl Pts',(0.00386794697500161,-0.15041563023346,
0.0897686143336374));
#17125=CARTESIAN_POINT('Ctrl Pts',(0.128476112576568,-0.0783184064825255,
0.0977076039709433));
#17126=CARTESIAN_POINT('Ctrl Pts',(0.135473254782295,0.0654742669580799,
0.105646593608249));
#17127=CARTESIAN_POINT('Ctrl Pts',(0.0184538891044151,0.149329569763132,
0.113585583245555));
#17128=CARTESIAN_POINT('Ctrl Pts',(-0.115458732720671,0.096483973363118,
0.12152457288286));
#17129=CARTESIAN_POINT('Ctrl Pts',(-0.143676805334049,-0.0446861343604874,
0.129463562520166));
#17130=CARTESIAN_POINT('Ctrl Pts',(-0.0403686054279526,-0.144949124289353,
0.137402552157472));
#17131=CARTESIAN_POINT('Ctrl Pts',(0.0998942839726139,-0.112521137758025,
0.145341541794778));
#17132=CARTESIAN_POINT('Ctrl Pts',(0.14871080372247,0.0229122455632766,
0.153280531432083));
#17133=CARTESIAN_POINT('Ctrl Pts',(0.0613927738894439,0.137371034794898,
0.161219521069389));
#17134=CARTESIAN_POINT('Ctrl Pts',(-0.0821261326059948,0.126076058196294,
0.169158510706695));
#17135=CARTESIAN_POINT('Ctrl Pts',(-0.150464193336327,-0.000632910110818063,
0.177097500344));
#17136=CARTESIAN_POINT('Ctrl Pts',(-0.0810625969653723,-0.126762492068094,
0.185036489981306));
#17137=CARTESIAN_POINT('Ctrl Pts',(0.0625462512992226,-0.136849700411639,
0.192975479618612));
#17138=CARTESIAN_POINT('Ctrl Pts',(0.148898293097928,-0.0216603868066741,
0.200914469255917));
#17139=CARTESIAN_POINT('Ctrl Pts',(0.0989441522193119,0.113357526360621,
0.208853458893223));
#17140=CARTESIAN_POINT('Ctrl Pts',(-0.0415865789238149,0.144604393083411,
0.216792448530529));
#17141=CARTESIAN_POINT('Ctrl Pts',(-0.144047647180085,0.0434758483035601,
0.224731438167835));
#17142=CARTESIAN_POINT('Ctrl Pts',(-0.114642966671137,-0.0974518559926297,
0.232670427805141));
#17143=CARTESIAN_POINT('Ctrl Pts',(0.0197094928286333,-0.149169064945282,
0.240609417442446));
#17144=CARTESIAN_POINT('Ctrl Pts',(0.136019262424063,-0.0643322181611298,
0.248548407079752));
#17145=CARTESIAN_POINT('Ctrl Pts',(0.127812719278849,0.0793963653730636,
0.256487396717058));
#17146=CARTESIAN_POINT('Ctrl Pts',(0.00260239121171357,0.150443017797356,
0.264426386354363));
#17147=CARTESIAN_POINT('Ctrl Pts',(-0.124990247656303,0.0837693979610897,
0.272365375991669));
#17148=CARTESIAN_POINT('Ctrl Pts',(-0.138162880936044,-0.0595893646165358,
0.280304365628975));
#17149=CARTESIAN_POINT('Ctrl Pts',(-0.0248568656394851,-0.148398147813718,
0.288243355266281));
#17150=CARTESIAN_POINT('Ctrl Pts',(0.111203906597776,-0.101358597076653,
0.296182344903586));
#17151=CARTESIAN_POINT('Ctrl Pts',(0.145465123646218,0.0384678027257296,
0.304121334540892));
#17152=CARTESIAN_POINT('Ctrl Pts',(0.0465629893725541,0.143079565503422,
0.312060324178198));
#17153=CARTESIAN_POINT('Ctrl Pts',(-0.0949643705016135,0.116711791945748,
0.319999313815503));
#17154=CARTESIAN_POINT('Ctrl Pts',(-0.149558357514911,-0.0164976283567656,
0.327938303452809));
#17155=CARTESIAN_POINT('Ctrl Pts',(-0.0672419181269484,-0.134604600554976,
0.335877293090115));
#17156=CARTESIAN_POINT('Ctrl Pts',(0.0766298889166206,-0.12949028600085,
0.343816282727421));
#17157=CARTESIAN_POINT('Ctrl Pts',(0.150352284446295,-0.00583648916182633,
0.351755272364726));
#17158=CARTESIAN_POINT('Ctrl Pts',(0.0864374678803939,0.123160213504125,
0.359694262002032));
#17159=CARTESIAN_POINT('Ctrl Pts',(-0.0566049265834532,0.139412181427728,
0.367633251639338));
#17160=CARTESIAN_POINT('Ctrl Pts',(-0.147829390149123,0.0280418517950267,
0.375572241276644));
#17161=CARTESIAN_POINT('Ctrl Pts',(-0.103726178443039,-0.108998871322406,
0.383511230913949));
#17162=CARTESIAN_POINT('Ctrl Pts',(0.0353312408083745,-0.146258597924691,
0.391450220551255));
#17163=CARTESIAN_POINT('Ctrl Pts',(0.142045330507792,-0.0496286018832686,
0.399389210188561));
#17164=CARTESIAN_POINT('Ctrl Pts',(0.118726655129599,0.0924329779120693,
0.407328199825866));
#17165=CARTESIAN_POINT('Ctrl Pts',(-0.0132781361506635,0.1498785012746,
0.415267189463172));
#17166=CARTESIAN_POINT('Ctrl Pts',(-0.133127703795094,0.0701205285647604,
0.423206179100478));
#17167=CARTESIAN_POINT('Ctrl Pts',(-0.131107982452518,-0.0738279823724454,
0.431145168737783));
#17168=CARTESIAN_POINT('Ctrl Pts',(-0.00906788859151817,-0.150192035209753,
0.439084158375089));
#17169=CARTESIAN_POINT('Ctrl Pts',(0.121273235812024,-0.0890655731449414,
0.447023148012395));
#17170=CARTESIAN_POINT('Ctrl Pts',(0.14059702422731,0.0535943170716914,
0.4549621376497));
#17171=CARTESIAN_POINT('Ctrl Pts',(0.031213872705855,0.14719228306762,0.462901127287006));
#17172=CARTESIAN_POINT('Ctrl Pts',(-0.106743440051405,0.106045801661112,
0.470840116924312));
#17173=CARTESIAN_POINT('Ctrl Pts',(-0.146984449047318,-0.0321783433727119,
0.478779106561618));
#17174=CARTESIAN_POINT('Ctrl Pts',(-0.0526712684425847,-0.140945420374714,
0.486718096198923));
#17175=CARTESIAN_POINT('Ctrl Pts',(0.0898588486235595,-0.120686624644175,
0.49465708583623));
#17176=CARTESIAN_POINT('Ctrl Pts',(0.150129348203927,0.0100525047535443,
0.502596075473534));
#17177=CARTESIAN_POINT('Ctrl Pts',(0.0729667185397875,0.131589254992538,
0.510535065110842));
#17178=CARTESIAN_POINT('Ctrl Pts',(-0.0709919412117167,0.132665060686482,
0.518474054748145));
#17179=CARTESIAN_POINT('Ctrl Pts',(-0.149962344179375,0.0122950954523496,
0.526413044385453));
#17180=CARTESIAN_POINT('Ctrl Pts',(-0.0916524986414713,-0.119330187030486,
0.534352034022757));
#17181=CARTESIAN_POINT('Ctrl Pts',(0.0505589280467443,-0.141716861518734,
0.542291023660064));
#17182=CARTESIAN_POINT('Ctrl Pts',(0.146487121137799,-0.0343714617774037,
0.550230013297369));
#17183=CARTESIAN_POINT('Ctrl Pts',(0.108316394245265,0.104438655591022,
0.558169002934674));
#17184=CARTESIAN_POINT('Ctrl Pts',(-0.0290105681715044,0.147642341414387,
0.566107992571982));
#17185=CARTESIAN_POINT('Ctrl Pts',(-0.139780343651344,0.0556895822633619,
0.574046982209285));
#17186=CARTESIAN_POINT('Ctrl Pts',(-0.122590794290966,-0.0872431727934394,
0.581985971846593));
#17187=CARTESIAN_POINT('Ctrl Pts',(0.00682222554696161,-0.150310782322966,
0.589924961483898));
#17188=CARTESIAN_POINT('Ctrl Pts',(0.129989965454297,-0.0757791721064987,
0.597863951121203));
#17189=CARTESIAN_POINT('Ctrl Pts',(0.134160800782372,0.0681230766876274,
0.60580294075851));
#17190=CARTESIAN_POINT('Ctrl Pts',(0.015516617634347,0.149663317553585,
0.613741930395814));
#17191=CARTESIAN_POINT('Ctrl Pts',(-0.117331965534667,0.0941970482962578,
0.621680920033121));
#17192=CARTESIAN_POINT('Ctrl Pts',(-0.142771175541451,-0.0475001629309618,
0.629619909670426));
#17193=CARTESIAN_POINT('Ctrl Pts',(-0.0375131590877193,-0.145714230393655,
0.637558899307733));
#17194=CARTESIAN_POINT('Ctrl Pts',(0.102085583566124,-0.110536906379362,
0.645497888945037));
#17195=CARTESIAN_POINT('Ctrl Pts',(0.148231970847143,0.0258293798362968,
0.653436878582344));
#17196=CARTESIAN_POINT('Ctrl Pts',(0.0586821478180281,0.138550639014834,
0.661375868219649));
#17197=CARTESIAN_POINT('Ctrl Pts',(-0.0845871597882484,0.124438283670714,
0.669314857856955));
#17198=CARTESIAN_POINT('Ctrl Pts',(-0.150422719745043,-0.00358879206139753,
0.67725384749426));
#17199=CARTESIAN_POINT('Ctrl Pts',(-0.078556588917505,-0.128330574617282,
0.685192837131567));
#17200=CARTESIAN_POINT('Ctrl Pts',(0.065222715229363,-0.135594511179713,
0.693131826768872));
#17201=CARTESIAN_POINT('Ctrl Pts',(0.149295093588351,-0.0187309656558678,
0.701070816406178));
#17202=CARTESIAN_POINT('Ctrl Pts',(0.0966980456281902,0.11527949520901,
0.709009806043483));
#17203=CARTESIAN_POINT('Ctrl Pts',(-0.044419435954706,0.14375947882982,
0.716948795680789));
#17204=CARTESIAN_POINT('Ctrl Pts',(-0.144873968183829,0.0406375120624596,
0.724887785318095));
#17205=CARTESIAN_POINT('Ctrl Pts',(-0.112706311402131,-0.099685311927494,
0.732826774955401));
#17206=CARTESIAN_POINT('Ctrl Pts',(0.0226362492002416,-0.148753064728429,
0.740765764592706));
#17207=CARTESIAN_POINT('Ctrl Pts',(0.137256875023267,-0.0616475814838108,
0.748704754230013));
#17208=CARTESIAN_POINT('Ctrl Pts',(0.126228238590478,0.0818920376245527,
0.756643743867318));
#17209=CARTESIAN_POINT('Ctrl Pts',(-0.000353699285724532,0.150465108715513,
0.764582733504624));
#17210=CARTESIAN_POINT('Ctrl Pts',(-0.126611849706441,0.0812976848247803,
0.772521723141928));
#17211=CARTESIAN_POINT('Ctrl Pts',(-0.136965528997667,-0.0622921978288208,
0.780460712779236));
#17212=CARTESIAN_POINT('Ctrl Pts',(-0.0219366533522686,-0.148857842533265,
0.788399702416541));
#17213=CARTESIAN_POINT('Ctrl Pts',(0.113173725020093,-0.0991543342927188,
0.796338692053846));
#17214=CARTESIAN_POINT('Ctrl Pts',(0.144681314438483,0.0413181715024817,
0.804277681691154));
#17215=CARTESIAN_POINT('Ctrl Pts',(0.0437430761464933,0.143966723006387,
0.812216671328456));
#17216=CARTESIAN_POINT('Ctrl Pts',(-0.0972389504488157,0.114823606281847,
0.820155660965765));
#17217=CARTESIAN_POINT('Ctrl Pts',(-0.149205382128735,-0.0194326526180533,
0.828094650603069));
#17218=CARTESIAN_POINT('Ctrl Pts',(-0.0645845121824554,-0.135899649852787,
0.836033640240376));
#17219=CARTESIAN_POINT('Ctrl Pts',(0.0791590524011713,-0.127959831458565,
0.843972629877681));
#17220=CARTESIAN_POINT('Ctrl Pts',(0.150437929635691,-0.00288155702400619,
0.851911619514986));
#17221=CARTESIAN_POINT('Ctrl Pts',(0.0840011924733913,0.12483458538003,
0.859850609152293));
#17222=CARTESIAN_POINT('Ctrl Pts',(-0.0593328794206009,0.138273220341526,
0.867789598789597));
#17223=CARTESIAN_POINT('Ctrl Pts',(-0.148351766552825,0.0251321985630355,
0.875728588426904));
#17224=CARTESIAN_POINT('Ctrl Pts',(-0.1015647786165,-0.111015628577859,
0.883667578064211));
#17225=CARTESIAN_POINT('Ctrl Pts',(0.0381978034543637,-0.145536256153639,
0.891606567701514));
#17226=CARTESIAN_POINT('Ctrl Pts',(0.142992914329196,-0.046828415471795,
0.899545557338823));
#17227=CARTESIAN_POINT('Ctrl Pts',(0.116887812080083,0.0947476302135675,
0.907484546976125));
#17228=CARTESIAN_POINT('Ctrl Pts',(-0.0162200712834111,0.149588713917584,
0.915423536613434));
#17229=CARTESIAN_POINT('Ctrl Pts',(-0.134479591021026,0.067491582014154,
0.923362526250738));
#17230=CARTESIAN_POINT('Ctrl Pts',(-0.129632261667175,-0.0763894677230377,
0.931301515888044));
#17231=CARTESIAN_POINT('Ctrl Pts',(-0.00611548103612966,-0.150341195071919,
0.93924050552535));
#17232=CARTESIAN_POINT('Ctrl Pts',(0.122999603362204,-0.0866658618874593,
0.947179495162656));
#17233=CARTESIAN_POINT('Ctrl Pts',(0.139516980595786,0.0563461282555487,
0.95511848479996));
#17234=CARTESIAN_POINT('Ctrl Pts',(0.0283161238170646,0.147777099632969,
0.963057474437267));
#17235=CARTESIAN_POINT('Ctrl Pts',(-0.108806203685475,0.103928264122473,
0.970996464074573));
#17236=CARTESIAN_POINT('Ctrl Pts',(-0.146323908690103,-0.0350597745230392,
0.978935453711877));
#17237=CARTESIAN_POINT('Ctrl Pts',(-0.049892103521326,-0.14195299239598,
0.986874443349185));
#17238=CARTESIAN_POINT('Ctrl Pts',(0.0922125030920605,-0.118897974404329,
0.994813432986488));
#17239=CARTESIAN_POINT('Ctrl Pts',(0.149902882860231,0.0129999905441286,
1.0027524226238));
#17240=CARTESIAN_POINT('Ctrl Pts',(0.0703674468853664,0.132997355096976,
1.0106914122611));
#17241=CARTESIAN_POINT('Ctrl Pts',(-0.0735845641169637,0.131244755962562,
1.01863040189841));
#17242=CARTESIAN_POINT('Ctrl Pts',(-0.150174949749745,0.00934657753497952,
1.02656939153571));
#17243=CARTESIAN_POINT('Ctrl Pts',(-0.0892904610481016,-0.121107752063083,
1.03450838117302));
#17244=CARTESIAN_POINT('Ctrl Pts',(0.0533333252681307,-0.140696234703703,
1.04244737081032));
#17245=CARTESIAN_POINT('Ctrl Pts',(0.147134107472884,-0.031486957015783,
1.05038636044763));
#17246=CARTESIAN_POINT('Ctrl Pts',(0.106243698045146,0.106546471877992,
1.05832535008494));
#17247=CARTESIAN_POINT('Ctrl Pts',(-0.0319055355867657,0.147043907874068,
1.06626433972224));
#17248=CARTESIAN_POINT('Ctrl Pts',(-0.14084743801815,0.0529327237885883,
1.07420332935955));
#17249=CARTESIAN_POINT('Ctrl Pts',(-0.120853163849259,-0.0896347412088629,
1.08214231899685));
#17250=CARTESIAN_POINT('Ctrl Pts',(0.00977389921538986,-0.150147743699608,
1.09008130863416));
#17251=CARTESIAN_POINT('Ctrl Pts',(0.13145362739741,-0.0732107771302755,
1.09802029827146));
#17252=CARTESIAN_POINT('Ctrl Pts',(0.132796568802552,0.0707456384395876,
1.10595928790877));
#17253=CARTESIAN_POINT('Ctrl Pts',(0.0125733526121963,0.149939270533256,
1.11389827754607));
#17254=CARTESIAN_POINT('Ctrl Pts',(-0.119159906186493,0.0918737764630459,
1.12183726718338));
#17255=CARTESIAN_POINT('Ctrl Pts',(-0.141810437433163,-0.0502958634379693,
1.12977625682069));
#17256=CARTESIAN_POINT('Ctrl Pts',(-0.0346432321137694,-0.146423087362162,
1.13771524645799));
#17257=CARTESIAN_POINT('Ctrl Pts',(0.104237477950025,-0.108510009835838,
1.1456542360953));
#17258=CARTESIAN_POINT('Ctrl Pts',(0.147695920811486,0.0287365450185451,
1.1535932257326));
#17259=CARTESIAN_POINT('Ctrl Pts',(0.0559488704325515,0.139676762352502,
1.16153221536991));
#17260=CARTESIAN_POINT('Ctrl Pts',(-0.0870155364008756,0.12275247642644,
1.16947120500722));
#17261=CARTESIAN_POINT('Ctrl Pts',(-0.150323183223479,-0.00654328889139735,
1.17741019464452));
#17262=CARTESIAN_POINT('Ctrl Pts',(-0.0760202581255566,-0.129849121670035,
1.18534918428183));
#17263=CARTESIAN_POINT('Ctrl Pts',(0.0678740032777675,-0.134286982701248,
1.19328817391913));
#17264=CARTESIAN_POINT('Ctrl Pts',(0.149634266389533,-0.0157943143574443,
1.20122716355644));
#17265=CARTESIAN_POINT('Ctrl Pts',(0.0944146137277022,0.117156966325547,
1.20916615319374));
#17266=CARTESIAN_POINT('Ctrl Pts',(-0.047235147145783,0.142859073628774,
1.21710514283105));
#17267=CARTESIAN_POINT('Ctrl Pts',(-0.145644368043342,0.037783489796601,
1.22504413246835));
#17268=CARTESIAN_POINT('Ctrl Pts',(-0.11072615165767,-0.101880289472715,
1.23298312210566));
#17269=CARTESIAN_POINT('Ctrl Pts',(0.0255542680118797,-0.148279646041953,
1.24092211174296));
#17270=CARTESIAN_POINT('Ctrl Pts',(0.138441506664824,-0.0589391489276913,
1.24886110138027));
#17271=CARTESIAN_POINT('Ctrl Pts',(0.124595033982396,0.0843560996663564,
1.25680009101758));
#17272=CARTESIAN_POINT('Ctrl Pts',(-0.00330965325590636,0.150429120316621,
1.26473908065488));
#17273=CARTESIAN_POINT('Ctrl Pts',(-0.128184579763139,0.0787945908985174,
1.27267807029219));
#17274=CARTESIAN_POINT('Ctrl Pts',(-0.135715308561414,-0.0649709863423027,
1.2806170599295));
#17275=CARTESIAN_POINT('Ctrl Pts',(-0.0190079735469551,-0.149260078337129,
1.2885560495668));
#17276=CARTESIAN_POINT('Ctrl Pts',(0.115099858543875,-0.0969117980795561,
1.29649503920411));
#17277=CARTESIAN_POINT('Ctrl Pts',(0.143841658454547,0.0441525915281748,
1.30443402884141));
#17278=CARTESIAN_POINT('Ctrl Pts',(0.0409062781470196,0.144798309552134,
1.31237301847872));
#17279=CARTESIAN_POINT('Ctrl Pts',(-0.0994759962839106,0.112891098884786,
1.32031200811602));
#17280=CARTESIAN_POINT('Ctrl Pts',(-0.148794813708878,-0.0223601759313527,
1.32825099775333));
#17281=CARTESIAN_POINT('Ctrl Pts',(-0.0619021766503053,-0.13714224202644,
1.33618998739064));
#17282=CARTESIAN_POINT('Ctrl Pts',(0.0816576604940555,-0.126379984705639,
1.34412897702794));
#17283=CARTESIAN_POINT('Ctrl Pts',(0.150465506209006,7.4487583413377E-5,
1.35206796666525));
#17284=CARTESIAN_POINT('Ctrl Pts',(0.0815324923277053,0.126460770918471,
1.36000695630255));
#17285=CARTESIAN_POINT('Ctrl Pts',(-0.062037929094705,0.137080886684378,
1.36794594593986));
#17286=CARTESIAN_POINT('Ctrl Pts',(-0.148816880822527,0.0222128430196456,
1.37588493557716));
#17287=CARTESIAN_POINT('Ctrl Pts',(-0.0993641722043223,-0.112989531455785,
1.38382392521447));
#17288=CARTESIAN_POINT('Ctrl Pts',(0.0410496166270677,-0.144757742348562,
1.39176291485178));
#17289=CARTESIAN_POINT('Ctrl Pts',(0.143885312916173,-0.0440101443352923,
1.39970190448908));
#17290=CARTESIAN_POINT('Ctrl Pts',(0.115003831846793,0.0970256929337524,
1.40764089412639));
#17291=CARTESIAN_POINT('Ctrl Pts',(-0.0191557100743377,0.149241218055048,
1.41557988376369));
#17292=CARTESIAN_POINT('Ctrl Pts',(-0.135779636557791,0.0648365220611291,
1.423518873401));
#17293=CARTESIAN_POINT('Ctrl Pts',(-0.128106375355825,-0.0789213496179777,
1.4314578630383));
#17294=CARTESIAN_POINT('Ctrl Pts',(-0.00316095527563228,-0.150432546011701,
1.43939685267561));
#17295=CARTESIAN_POINT('Ctrl Pts',(0.12467895337041,-0.0842322751882648,
1.44733584231291));
#17296=CARTESIAN_POINT('Ctrl Pts',(0.138382210043398,0.0590753877074232,
1.45527483195022));
#17297=CARTESIAN_POINT('Ctrl Pts',(0.0254091034322018,0.148306397458819,
1.46321382158753));
#17298=CARTESIAN_POINT('Ctrl Pts',(-0.110830116988615,0.101767718932792,
1.47115281122483));
#17299=CARTESIAN_POINT('Ctrl Pts',(-0.145600909330124,-0.0379221829034233,
1.47909180086214));
#17300=CARTESIAN_POINT('Ctrl Pts',(-0.0471050325108872,-0.142916194795756,
1.48703079049945));
#17301=CARTESIAN_POINT('Ctrl Pts',(0.0945521370959566,-0.117043625665234,
1.49496978013675));
#17302=CARTESIAN_POINT('Ctrl Pts',(0.14957741911039,0.0159047428854941,
1.50290876977406));
#17303=CARTESIAN_POINT('Ctrl Pts',(0.0678206238522695,0.134426714629862,
1.51084775941136));
#17304=CARTESIAN_POINT('Ctrl Pts',(-0.0763126473618499,0.129627546381738,
1.51878674904867));
#17305=CARTESIAN_POINT('Ctrl Pts',(-0.125385920115907,0.0477050348167321,
1.52407940880687));
#17306=CARTESIAN_POINT('Ctrl Pts',(-0.127184992207234,0.00540996832206346,
1.52672573868597));
#17307=CARTESIAN_POINT('Ctrl Pts',(0.0684664424539414,-0.095829519891843,
-1.38777878078145E-17));
#17308=CARTESIAN_POINT('Ctrl Pts',(0.100334321247169,-0.0730611673843044,
0.00264632987910189));
#17309=CARTESIAN_POINT('Ctrl Pts',(0.139021564822767,0.00636891437108143,
0.00793898963730573));
#17310=CARTESIAN_POINT('Ctrl Pts',(0.0699018669780613,0.120491966796142,
0.0158779792746114));
#17311=CARTESIAN_POINT('Ctrl Pts',(-0.0632645460347191,0.123954346655885,
0.0238169689119172));
#17312=CARTESIAN_POINT('Ctrl Pts',(-0.138486976988987,0.0141253725679007,
0.0317559585492228));
#17313=CARTESIAN_POINT('Ctrl Pts',(-0.0869496735326521,-0.108728403071097,
0.0396949481865287));
#17314=CARTESIAN_POINT('Ctrl Pts',(0.0441923146003338,-0.131999388615902,
0.0476339378238343));
#17315=CARTESIAN_POINT('Ctrl Pts',(0.134874939024977,-0.034459980695041,
0.0555729274611401));
#17316=CARTESIAN_POINT('Ctrl Pts',(0.102091080224759,0.094638871230671,
0.0635119170984456));
#17317=CARTESIAN_POINT('Ctrl Pts',(-0.0241513666277066,0.137095110112719,
0.0714509067357516));
#17318=CARTESIAN_POINT('Ctrl Pts',(-0.128284260007319,0.0540539703915629,
0.0793898963730571));
#17319=CARTESIAN_POINT('Ctrl Pts',(-0.114982038412656,-0.0784718756714057,
0.0873288860103631));
#17320=CARTESIAN_POINT('Ctrl Pts',(0.00357853460314598,-0.139161043603659,
0.0952678756476685));
#17321=CARTESIAN_POINT('Ctrl Pts',(0.118863112008681,-0.0724583686054966,
0.103206865284975));
#17322=CARTESIAN_POINT('Ctrl Pts',(0.125336705278751,0.0605752693714656,
0.11114585492228));
#17323=CARTESIAN_POINT('Ctrl Pts',(0.0170731091066207,0.138156245709763,
0.119084844559586));
#17324=CARTESIAN_POINT('Ctrl Pts',(-0.106819734848208,0.0892647286947484,
0.127023834196891));
#17325=CARTESIAN_POINT('Ctrl Pts',(-0.132926439498961,-0.0413425724611633,
0.134962823834197));
#17326=CARTESIAN_POINT('Ctrl Pts',(-0.0373480950846616,-0.134103559412242,
0.142901813471503));
#17327=CARTESIAN_POINT('Ctrl Pts',(0.0924198687735613,-0.104101940294199,
0.150840803108809));
#17328=CARTESIAN_POINT('Ctrl Pts',(0.137583777756591,0.0211978768359354,
0.158779792746114));
#17329=CARTESIAN_POINT('Ctrl Pts',(0.0567991668878991,0.127092487218924,
0.16671878238342));
#17330=CARTESIAN_POINT('Ctrl Pts',(-0.075981188277068,0.116642637502503,
0.174657772020726));
#17331=CARTESIAN_POINT('Ctrl Pts',(-0.139205973057234,-0.000585553717998882,
0.182596761658032));
#17332=CARTESIAN_POINT('Ctrl Pts',(-0.0749972298318695,-0.11727771015962,
0.190535751295337));
#17333=CARTESIAN_POINT('Ctrl Pts',(0.0578663373665801,-0.126610160769685,
0.198474740932643));
#17334=CARTESIAN_POINT('Ctrl Pts',(0.13775723856723,-0.0200396862227523,
0.206413730569949));
#17335=CARTESIAN_POINT('Ctrl Pts',(0.091540828968026,0.104875747581476,
0.214352720207254));
#17336=CARTESIAN_POINT('Ctrl Pts',(-0.0384749358425138,0.133784622116252,
0.22229170984456));
#17337=CARTESIAN_POINT('Ctrl Pts',(-0.133269533752038,0.0402228439430644,
0.230230699481866));
#17338=CARTESIAN_POINT('Ctrl Pts',(-0.106065007067505,-0.0901601911982067,
0.238169689119172));
#17339=CARTESIAN_POINT('Ctrl Pts',(0.0182347644767634,-0.138007750384372,
0.246108678756477));
#17340=CARTESIAN_POINT('Ctrl Pts',(0.125841858853055,-0.0595186723796334,
0.254047668393783));
#17341=CARTESIAN_POINT('Ctrl Pts',(0.118249355954961,0.073455671106145,
0.261986658031089));
#17342=CARTESIAN_POINT('Ctrl Pts',(0.00240767183786234,0.139186381940956,
0.269925647668394));
#17343=CARTESIAN_POINT('Ctrl Pts',(-0.115638070838342,0.0775014991741366,
0.277864637305701));
#17344=CARTESIAN_POINT('Ctrl Pts',(-0.12782508485658,-0.0551306945617612,
0.285803626943006));
#17345=CARTESIAN_POINT('Ctrl Pts',(-0.0229969941138309,-0.137294515779738,
0.293742616580312));
#17346=CARTESIAN_POINT('Ctrl Pts',(0.102883268653204,-0.0937746172089793,
0.301681606217617));
#17347=CARTESIAN_POINT('Ctrl Pts',(0.134580950019115,0.0355895166223291,
0.309620595854923));
#17348=CARTESIAN_POINT('Ctrl Pts',(0.0430789950773988,0.13237388709478,
0.317559585492229));
#17349=CARTESIAN_POINT('Ctrl Pts',(-0.0878588274613298,0.107979036106918,
0.325498575129534));
#17350=CARTESIAN_POINT('Ctrl Pts',(-0.1383679148179,-0.0152632221501787,
0.33343756476684));
#17351=CARTESIAN_POINT('Ctrl Pts',(-0.0622106591311991,-0.12453304658572,
0.341376554404146));
#17352=CARTESIAN_POINT('Ctrl Pts',(0.0708961914151981,-0.119801401679107,
0.349315544041452));
#17353=CARTESIAN_POINT('Ctrl Pts',(0.1391024375543,-0.00539978406154301,
0.357254533678757));
#17354=CARTESIAN_POINT('Ctrl Pts',(0.0799699354250877,0.113944965792994,
0.365193523316063));
#17355=CARTESIAN_POINT('Ctrl Pts',(-0.0523695618881846,0.128980908622551,
0.373132512953369));
#17356=CARTESIAN_POINT('Ctrl Pts',(-0.136768314413298,0.0259436692471295,
0.381071502590675));
#17357=CARTESIAN_POINT('Ctrl Pts',(-0.0959650484377783,-0.100843221288265,
0.38901049222798));
#17358=CARTESIAN_POINT('Ctrl Pts',(0.0326876424682324,-0.135315053971568,
0.396949481865287));
#17359=CARTESIAN_POINT('Ctrl Pts',(0.13141703692502,-0.0459152284901983,
0.404888471502591));
#17360=CARTESIAN_POINT('Ctrl Pts',(0.109843140674695,0.0855168418978295,
0.412827461139898));
#17361=CARTESIAN_POINT('Ctrl Pts',(-0.0122846228212416,0.13866410438033,
0.420766450777203));
#17362=CARTESIAN_POINT('Ctrl Pts',(-0.123166656044517,0.0648738825743514,
0.428705440414509));
#17363=CARTESIAN_POINT('Ctrl Pts',(-0.121298056821252,-0.0683039326309071,
0.436644430051815));
#17364=CARTESIAN_POINT('Ctrl Pts',(-0.00838939967687663,-0.138954178686792,
0.44458341968912));
#17365=CARTESIAN_POINT('Ctrl Pts',(0.11219917790857,-0.0824013973067221,
0.452522409326426));
#17366=CARTESIAN_POINT('Ctrl Pts',(0.13007709763057,0.0495842159710775,
0.460461398963732));
#17367=CARTESIAN_POINT('Ctrl Pts',(0.0288783492374893,0.136178877755608,
0.468400388601037));
#17368=CARTESIAN_POINT('Ctrl Pts',(-0.0987565487199846,0.0981111099028881,
0.476339378238344));
#17369=CARTESIAN_POINT('Ctrl Pts',(-0.135986594552616,-0.0297706550724338,
0.484278367875649));
#17370=CARTESIAN_POINT('Ctrl Pts',(-0.0487302328423073,-0.130399425645183,
0.492217357512954));
#17371=CARTESIAN_POINT('Ctrl Pts',(0.0831353173341669,-0.111656458896056,
0.50015634715026));
#17372=CARTESIAN_POINT('Ctrl Pts',(0.13889618212661,0.00930034365552528,
0.508095336787567));
#17373=CARTESIAN_POINT('Ctrl Pts',(0.0675071113591811,0.12174331898465,
0.516034326424871));
#17374=CARTESIAN_POINT('Ctrl Pts',(-0.0656800932930844,0.122738629397884,
0.523973316062178));
#17375=CARTESIAN_POINT('Ctrl Pts',(-0.138741673886299,0.0113751364249866,
0.531912305699483));
#17376=CARTESIAN_POINT('Ctrl Pts',(-0.0847947606245053,-0.110401514355972,
0.539851295336789));
#17377=CARTESIAN_POINT('Ctrl Pts',(0.0467759446245483,-0.131113145053959,
0.547790284974095));
#17378=CARTESIAN_POINT('Ctrl Pts',(0.135526478334676,-0.031799677225719,
0.555729274611401));
#17379=CARTESIAN_POINT('Ctrl Pts',(0.100211809365564,0.0966242157284558,
0.563668264248707));
#17380=CARTESIAN_POINT('Ctrl Pts',(-0.0268399031138932,0.136595261273209,
0.571607253886012));
#17381=CARTESIAN_POINT('Ctrl Pts',(-0.129321523751272,0.0515227066069736,
0.579546243523318));
#17382=CARTESIAN_POINT('Ctrl Pts',(-0.113418152377209,-0.0807153548762533,
0.587485233160623));
#17383=CARTESIAN_POINT('Ctrl Pts',(0.00631176444456456,-0.139064040754811,
0.595424222797929));
#17384=CARTESIAN_POINT('Ctrl Pts',(0.120263693490807,-0.0701091280034811,
0.603363212435234));
#17385=CARTESIAN_POINT('Ctrl Pts',(0.124122453355413,0.0630258865426945,
0.611302202072541));
#17386=CARTESIAN_POINT('Ctrl Pts',(0.0143556138404206,0.138465021405133,
0.619241191709845));
#17387=CARTESIAN_POINT('Ctrl Pts',(-0.108552806291007,0.0871489187988374,
0.627180181347153));
#17388=CARTESIAN_POINT('Ctrl Pts',(-0.132088571872698,-0.043946046262323,
0.635119170984457));
#17389=CARTESIAN_POINT('Ctrl Pts',(-0.0347063025259737,-0.134811417789573,
0.643058160621763));
#17390=CARTESIAN_POINT('Ctrl Pts',(0.0944472082050275,-0.102266175560326,
0.65099715025907));
#17391=CARTESIAN_POINT('Ctrl Pts',(0.137140772714236,0.0238967416356601,
0.658936139896373));
#17392=CARTESIAN_POINT('Ctrl Pts',(0.054291358674537,0.128183829614862,
0.666875129533682));
#17393=CARTESIAN_POINT('Ctrl Pts',(-0.0782580734018908,0.115127406593233,
0.674814119170985));
#17394=CARTESIAN_POINT('Ctrl Pts',(-0.139167602654929,-0.00332026696803425,
0.682753108808293));
#17395=CARTESIAN_POINT('Ctrl Pts',(-0.0726787294560835,-0.118728463672822,
0.690692098445597));
#17396=CARTESIAN_POINT('Ctrl Pts',(0.0603425395611779,-0.125448888878168,
0.698631088082904));
#17397=CARTESIAN_POINT('Ctrl Pts',(0.138124349154501,-0.0173294538893964,
0.706570077720209));
#17398=CARTESIAN_POINT('Ctrl Pts',(0.0894627833767505,0.106653908470079,
0.714509067357515));
#17399=CARTESIAN_POINT('Ctrl Pts',(-0.0410958292974484,0.133002927094911,
0.72244805699482));
#17400=CARTESIAN_POINT('Ctrl Pts',(-0.134034026730954,0.0375968812502473,
0.730387046632127));
#17401=CARTESIAN_POINT('Ctrl Pts',(-0.104273258644039,-0.0922265326964679,
0.738326036269432));
#17402=CARTESIAN_POINT('Ctrl Pts',(0.0209425314183671,-0.137622876656644,
0.746265025906738));
#17403=CARTESIAN_POINT('Ctrl Pts',(0.126986869252672,-0.0570349089493802,
0.754204015544043));
#17404=CARTESIAN_POINT('Ctrl Pts',(0.11678343126468,0.0757646090434518,
0.762143005181349));
#17405=CARTESIAN_POINT('Ctrl Pts',(-0.000327234354877375,0.139206819944772,
0.770081994818654));
#17406=CARTESIAN_POINT('Ctrl Pts',(-0.117138339349379,0.0752147276530931,
0.778020984455961));
#17407=CARTESIAN_POINT('Ctrl Pts',(-0.126717322684213,-0.0576312930030564,
0.785959974093266));
#17408=CARTESIAN_POINT('Ctrl Pts',(-0.0202952816069424,-0.137719814645367,
0.793898963730571));
#17409=CARTESIAN_POINT('Ctrl Pts',(0.104705698854998,-0.0917352845351548,
0.801837953367879));
#17410=CARTESIAN_POINT('Ctrl Pts',(0.133855787965376,0.0382266115373486,
0.809776943005182));
#17411=CARTESIAN_POINT('Ctrl Pts',(0.0404700769297216,0.133194664588195,
0.81771593264249));
#17412=CARTESIAN_POINT('Ctrl Pts',(-0.0899632159395838,0.106232130635072,
0.825654922279794));
#17413=CARTESIAN_POINT('Ctrl Pts',(-0.13804135019805,-0.0179786383510676,
0.833593911917101));
#17414=CARTESIAN_POINT('Ctrl Pts',(-0.059752088941783,-0.125731196083361,
0.841532901554406));
#17415=CARTESIAN_POINT('Ctrl Pts',(0.0732361146625898,-0.118385460722959,
0.849471891191712));
#17416=CARTESIAN_POINT('Ctrl Pts',(0.139181674492094,-0.00266594955618734,
0.857410880829018));
#17417=CARTESIAN_POINT('Ctrl Pts',(0.077715950067195,0.115494055719818,
0.865349870466323));
#17418=CARTESIAN_POINT('Ctrl Pts',(-0.0548934004223171,0.127927168308903,
0.87328886010363));
#17419=CARTESIAN_POINT('Ctrl Pts',(-0.137251604915624,0.0232517257326144,
0.881227849740934));
#17420=CARTESIAN_POINT('Ctrl Pts',(-0.0939653715754795,-0.102709078207047,
0.889166839378241));
#17421=CARTESIAN_POINT('Ctrl Pts',(0.0353397195745277,-0.134646760160997,
0.897105829015547));
#17422=CARTESIAN_POINT('Ctrl Pts',(0.132293719443212,-0.0433245611326863,
0.905044818652852));
#17423=CARTESIAN_POINT('Ctrl Pts',(0.108141885842356,0.0876583043865096,
0.912983808290157));
#17424=CARTESIAN_POINT('Ctrl Pts',(-0.0150064327997127,0.138395999855801,
0.920922797927463));
#17425=CARTESIAN_POINT('Ctrl Pts',(-0.124417390671652,0.0624416423544169,
0.928861787564769));
#17426=CARTESIAN_POINT('Ctrl Pts',(-0.119932754264349,-0.0706737593172073,
0.936800777202075));
#17427=CARTESIAN_POINT('Ctrl Pts',(-0.00565790085648466,-0.139092177922979,
0.944739766839381));
#17428=CARTESIAN_POINT('Ctrl Pts',(0.113796373024222,-0.0801812402497705,
0.952678756476687));
#17429=CARTESIAN_POINT('Ctrl Pts',(0.129077866376032,0.0521301276928276,
0.960617746113992));
#17430=CARTESIAN_POINT('Ctrl Pts',(0.026197419344502,0.13671993644362,0.968556735751298));
#17431=CARTESIAN_POINT('Ctrl Pts',(-0.100664969670515,0.0961520134094621,
0.976495725388603));
#17432=CARTESIAN_POINT('Ctrl Pts',(-0.13537547797311,-0.0324364881732178,
0.98443471502591));
#17433=CARTESIAN_POINT('Ctrl Pts',(-0.0461590140787468,-0.131331607851033,
0.992373704663214));
#17434=CARTESIAN_POINT('Ctrl Pts',(0.0853128637208732,-0.110001641284132,
1.00031269430052));
#17435=CARTESIAN_POINT('Ctrl Pts',(0.138686661656432,0.0120272889735618,
1.00825168393783));
#17436=CARTESIAN_POINT('Ctrl Pts',(0.0651023256631918,0.123046060459907,
1.01619067357513));
#17437=CARTESIAN_POINT('Ctrl Pts',(-0.0680787277209358,0.121424596492465,
1.02412966321244));
#17438=CARTESIAN_POINT('Ctrl Pts',(-0.138938371616466,0.00864723620724691,
1.03206865284975));
#17439=CARTESIAN_POINT('Ctrl Pts',(-0.0826094583655966,-0.112046076191904,
1.04000764248705));
#17440=CARTESIAN_POINT('Ctrl Pts',(0.0493427524230464,-0.130168884856471,
1.04794663212436));
#17441=CARTESIAN_POINT('Ctrl Pts',(0.136125055048066,-0.0291310004912345,
1.05588562176166));
#17442=CARTESIAN_POINT('Ctrl Pts',(0.0982941990358779,0.0985743183458784,
1.06382461139897));
#17443=CARTESIAN_POINT('Ctrl Pts',(-0.0295182596522469,0.136041604476578,
1.07176360103627));
#17444=CARTESIAN_POINT('Ctrl Pts',(-0.130308774647192,0.0489721252490281,
1.07970259067358));
#17445=CARTESIAN_POINT('Ctrl Pts',(-0.111810537096203,-0.0829279783650712,
1.08764158031088));
#17446=CARTESIAN_POINT('Ctrl Pts',(0.00904258428980543,-0.13891320121148,
1.09558056994819));
#17447=CARTESIAN_POINT('Ctrl Pts',(0.121617839487272,-0.067732908692211,
1.1035195595855));
#17448=CARTESIAN_POINT('Ctrl Pts',(0.122860297649024,0.0654522196953821,
1.1114585492228));
#17449=CARTESIAN_POINT('Ctrl Pts',(0.0116325734791967,0.138720326685422,
1.11939753886011));
#17450=CARTESIAN_POINT('Ctrl Pts',(-0.110243974478508,0.0849994817198388,
1.12733652849741));
#17451=CARTESIAN_POINT('Ctrl Pts',(-0.131199719314147,-0.0465325633653302,
1.13527551813472));
#17452=CARTESIAN_POINT('Ctrl Pts',(-0.0320511128216771,-0.13546723577438,
1.14321450777202));
#17453=CARTESIAN_POINT('Ctrl Pts',(0.0964380908528195,-0.100390938007982,
1.15115349740933));
#17454=CARTESIAN_POINT('Ctrl Pts',(0.136644831685568,0.0265863832644056,
1.15909248704664));
#17455=CARTESIAN_POINT('Ctrl Pts',(0.0517625939920979,0.129225692742072,
1.16703147668394));
#17456=CARTESIAN_POINT('Ctrl Pts',(-0.0805047509788913,0.113567736929491,
1.17497046632125));
#17457=CARTESIAN_POINT('Ctrl Pts',(-0.139075513779617,-0.00605369873671642,
1.18290945595855));
#17458=CARTESIAN_POINT('Ctrl Pts',(-0.0703321751825429,-0.12013338809653,
1.19084844559586));
#17459=CARTESIAN_POINT('Ctrl Pts',(0.0627954496153871,-0.124239193932754,
1.19878743523316));
#17460=CARTESIAN_POINT('Ctrl Pts',(0.138438143943654,-0.0146125323915816,
1.20672642487047));
#17461=CARTESIAN_POINT('Ctrl Pts',(0.0873502052771435,0.108390901091839,
1.21466541450777));
#17462=CARTESIAN_POINT('Ctrl Pts',(-0.043700859820065,0.132169893139269,
1.22260440414508));
#17463=CARTESIAN_POINT('Ctrl Pts',(-0.134746782767514,0.0349564062120582,
1.23054339378239));
#17464=CARTESIAN_POINT('Ctrl Pts',(-0.102441260891455,-0.0942572748833364,
1.23848238341969));
#17465=CARTESIAN_POINT('Ctrl Pts',(0.0236422145726536,-0.137184880695923,
1.246421373057));
#17466=CARTESIAN_POINT('Ctrl Pts',(0.128082862902196,-0.0545291301253663,
1.2543603626943));
#17467=CARTESIAN_POINT('Ctrl Pts',(0.115272428336817,0.0780443019497631,
1.26229935233161));
#17468=CARTESIAN_POINT('Ctrl Pts',(-0.00306201423577413,0.139173524314926,
1.27023834196891));
#17469=CARTESIAN_POINT('Ctrl Pts',(-0.118593392628464,0.0728989233548558,
1.27817733160622));
#17470=CARTESIAN_POINT('Ctrl Pts',(-0.125560647806918,-0.06010964584811,
1.28611632124353));
#17471=CARTESIAN_POINT('Ctrl Pts',(-0.0175857351491984,-0.138091953858251,
1.29405531088083));
#17472=CARTESIAN_POINT('Ctrl Pts',(0.106487712804436,-0.089660542174548,
1.30199430051814));
#17473=CARTESIAN_POINT('Ctrl Pts',(0.133078957772855,0.0408489510387311,
1.30993329015544));
#17474=CARTESIAN_POINT('Ctrl Pts',(0.0378455373822902,0.133964029124136,
1.31787227979275));
#17475=CARTESIAN_POINT('Ctrl Pts',(-0.0920328787300654,0.104444219726284,
1.32581126943006));
#17476=CARTESIAN_POINT('Ctrl Pts',(-0.137661501842601,-0.0206871148492911,
1.33375025906736));
#17477=CARTESIAN_POINT('Ctrl Pts',(-0.0572704544775333,-0.126880813469472,
1.34168924870467));
#17478=CARTESIAN_POINT('Ctrl Pts',(0.0755477687720905,-0.116923823242002,
1.34962823834197));
#17479=CARTESIAN_POINT('Ctrl Pts',(0.13920718769651,6.89141801743488E-5,
1.35756722797928));
#17480=CARTESIAN_POINT('Ctrl Pts',(0.0754319660950179,0.116998564767658,
1.36550621761658));
#17481=CARTESIAN_POINT('Ctrl Pts',(-0.0573960494825499,0.126824048933643,
1.37344520725389));
#17482=CARTESIAN_POINT('Ctrl Pts',(-0.13768191782304,0.0205508058651932,
1.38138419689119));
#17483=CARTESIAN_POINT('Ctrl Pts',(-0.0919294216917856,-0.104535287252199,
1.3893231865285));
#17484=CARTESIAN_POINT('Ctrl Pts',(0.0379781508110965,-0.133926497290667,
1.39726217616581));
#17485=CARTESIAN_POINT('Ctrl Pts',(0.133119345865688,-0.0407171622080862,
1.40520116580311));
#17486=CARTESIAN_POINT('Ctrl Pts',(0.106398871137127,0.0897659150453452,
1.41314015544042));
#17487=CARTESIAN_POINT('Ctrl Pts',(-0.0177224175491345,0.138074504763813,
1.42107914507772));
#17488=CARTESIAN_POINT('Ctrl Pts',(-0.125620162573399,0.0599852426217579,
1.42901813471503));
#17489=CARTESIAN_POINT('Ctrl Pts',(-0.118521039729242,-0.0730161975746823,
1.43695712435233));
#17490=CARTESIAN_POINT('Ctrl Pts',(-0.00292444232197888,-0.139176693688359,
1.44489611398964));
#17491=CARTESIAN_POINT('Ctrl Pts',(0.115350068603298,-0.0779297424218237,
1.45283510362695));
#17492=CARTESIAN_POINT('Ctrl Pts',(0.128028003046829,0.0546551750765237,
1.46077409326425));
#17493=CARTESIAN_POINT('Ctrl Pts',(0.0235079116789307,0.137209630484779,
1.46871308290156));
#17494=CARTESIAN_POINT('Ctrl Pts',(-0.102537447198224,0.0941531272373115,
1.47665207253886));
#17495=CARTESIAN_POINT('Ctrl Pts',(-0.134706575776555,-0.0350847218495708,
1.48459106217617));
#17496=CARTESIAN_POINT('Ctrl Pts',(-0.0435804807853106,-0.132222740314769,
1.49253005181348));
#17497=CARTESIAN_POINT('Ctrl Pts',(0.0874774386997331,-0.108286040948335,
1.50046904145078));
#17498=CARTESIAN_POINT('Ctrl Pts',(0.138385550162814,0.0147146982980264,
1.50840803108809));
#17499=CARTESIAN_POINT('Ctrl Pts',(0.0627460642121078,0.124368470664037,
1.51634702072539));
#17500=CARTESIAN_POINT('Ctrl Pts',(-0.0706026869052757,0.119928391791904,
1.5242860103627));
#17501=CARTESIAN_POINT('Ctrl Pts',(-0.116004137797729,0.0441355889673283,
1.5295786701209));
#17502=CARTESIAN_POINT('Ctrl Pts',(-0.117668597464313,0.00500517689812487,
1.532225));
#17503=CARTESIAN_POINT('',(0.0684664424539461,-0.0958295198918396,0.));
#17504=CARTESIAN_POINT('Ctrl Pts',(0.0684664424539414,-0.095829519891843,
-1.38777878078145E-17));
#17505=CARTESIAN_POINT('Ctrl Pts',(0.100334321247169,-0.0730611673843044,
0.00264632987910189));
#17506=CARTESIAN_POINT('Ctrl Pts',(0.139021564822767,0.00636891437108143,
0.00793898963730573));
#17507=CARTESIAN_POINT('Ctrl Pts',(0.0699018669780613,0.120491966796142,
0.0158779792746114));
#17508=CARTESIAN_POINT('Ctrl Pts',(-0.0632645460347191,0.123954346655885,
0.0238169689119172));
#17509=CARTESIAN_POINT('Ctrl Pts',(-0.11596266760442,0.0470121293552651,
0.0293787386625077));
#17510=CARTESIAN_POINT('Ctrl Pts',(-0.117944740497024,0.00404481602818191,
0.0322941785339964));
#17511=CARTESIAN_POINT('Ctrl Pts',(-0.117917485785546,7.60014832213644E-5,
0.0325632885263832));
#17512=CARTESIAN_POINT('Ctrl Pts',(0.0635546915223951,0.132092229195826,
-2.16840434497101E-19));
#17513=CARTESIAN_POINT('Ctrl Pts',(0.0668114782730532,0.13015255741457,
-1.00603861447787E-18));
#17514=CARTESIAN_POINT('Ctrl Pts',(0.0699821360194518,0.12808121947321,
-2.9262196004085E-17));
#17515=CARTESIAN_POINT('Ctrl Pts',(0.0730575207853233,0.125877721325919,
-2.71050543121376E-17));
#17516=CARTESIAN_POINT('Ctrl Pts',(0.0789281193465506,0.121671466161783,
-2.36378102375718E-17));
#17517=CARTESIAN_POINT('Ctrl Pts',(0.0844522091809674,0.11698398814956,
1.43782932504085E-18));
#17518=CARTESIAN_POINT('Ctrl Pts',(0.0895990070394484,0.111875963994554,
9.97465998686664E-18));
#17519=CARTESIAN_POINT('Ctrl Pts',(0.0928865546640729,0.108613183302742,
1.54276111490851E-17));
#17520=CARTESIAN_POINT('Ctrl Pts',(0.0960206821069302,0.105176950779614,
-2.53636710091701E-17));
#17521=CARTESIAN_POINT('Ctrl Pts',(0.098978417360439,0.101599719103904,
-1.56125112837913E-17));
#17522=CARTESIAN_POINT('Ctrl Pts',(0.103148772110026,0.0965558852815647,
-1.86354736740503E-18));
#17523=CARTESIAN_POINT('Ctrl Pts',(0.106976174326278,0.0912251680483688,
1.1337629845105E-17));
#17524=CARTESIAN_POINT('Ctrl Pts',(0.110435561611279,0.0856523061447448,
2.03830008427275E-17));
#17525=CARTESIAN_POINT('Ctrl Pts',(0.112407683932559,0.0824753373788608,
2.55395723911076E-17));
#17526=CARTESIAN_POINT('Ctrl Pts',(0.114261188142284,0.0792174064057451,
2.29308760465575E-17));
#17527=CARTESIAN_POINT('Ctrl Pts',(0.115986535786665,0.0758936579718971,
2.08166817117217E-17));
#17528=CARTESIAN_POINT('Ctrl Pts',(0.120573220307724,0.0670577659456877,
1.51962825639422E-17));
#17529=CARTESIAN_POINT('Ctrl Pts',(0.124235263225439,0.0578042025119142,
2.52358375750583E-18));
#17530=CARTESIAN_POINT('Ctrl Pts',(0.126883306113679,0.0482911783993335,
1.30104260698261E-17));
#17531=CARTESIAN_POINT('Ctrl Pts',(0.128478610866444,0.0425600882242624,
1.93281898253259E-17));
#17532=CARTESIAN_POINT('Ctrl Pts',(0.129704960854084,0.0367345196138549,
-5.78096029915021E-19));
#17533=CARTESIAN_POINT('Ctrl Pts',(0.130533291754837,0.0308494671050701,
0.));
#17534=CARTESIAN_POINT('Ctrl Pts',(0.131003715791213,0.0275072397983871,
3.2831114661813E-19));
#17535=CARTESIAN_POINT('Ctrl Pts',(0.131345346899704,0.0241444941465381,
-1.7128612844445E-18));
#17536=CARTESIAN_POINT('Ctrl Pts',(0.131551728167405,0.0207857616715298,
2.60208521396521E-18));
#17537=CARTESIAN_POINT('Ctrl Pts',(0.131851321606701,0.0159100565018035,
8.86587880453295E-18));
#17538=CARTESIAN_POINT('Ctrl Pts',(0.131867617692795,0.0110341713389591,
-1.68111772803455E-17));
#17539=CARTESIAN_POINT('Ctrl Pts',(0.131586936334964,0.0061777758930637,
-6.93889390390723E-18));
#17540=CARTESIAN_POINT('Ctrl Pts',(0.131099036368572,-0.00226395031615145,
9.98510028643051E-18));
#17541=CARTESIAN_POINT('Ctrl Pts',(0.129715139118287,-0.0106479390144509,
1.03491660509995E-17));
#17542=CARTESIAN_POINT('Ctrl Pts',(0.127493709984164,-0.018859987399606,
1.04083408558608E-17));
#17543=CARTESIAN_POINT('Ctrl Pts',(0.126553994220251,-0.0223338732882013,
1.04333731632617E-17));
#17544=CARTESIAN_POINT('Ctrl Pts',(0.125463061762623,-0.0257782540966497,
1.75224609115742E-17));
#17545=CARTESIAN_POINT('Ctrl Pts',(0.124232565886791,-0.0291638780753137,
1.73472347597681E-17));
#17546=CARTESIAN_POINT('Ctrl Pts',(0.12170396813588,-0.0361211392462112,
1.69871551674183E-17));
#17547=CARTESIAN_POINT('Ctrl Pts',(0.118582485980247,-0.0428512226170345,
-6.45748389186585E-19));
#17548=CARTESIAN_POINT('Ctrl Pts',(0.114911168983798,-0.0492778939609075,
3.46944695195361E-18));
#17549=CARTESIAN_POINT('Ctrl Pts',(0.112347970921096,-0.0537647937721124,
6.34254691478841E-18));
#17550=CARTESIAN_POINT('Ctrl Pts',(0.109516356061708,-0.0581036184196785,
-1.05628593522785E-17));
#17551=CARTESIAN_POINT('Ctrl Pts',(0.106427098863261,-0.0622637901458048,
-1.21430643318376E-17));
#17552=CARTESIAN_POINT('Ctrl Pts',(0.104287070791936,-0.0651456752410043,
-1.32377232732828E-17));
#17553=CARTESIAN_POINT('Ctrl Pts',(0.102021590876101,-0.067943056099314,
-1.03088264066386E-17));
#17554=CARTESIAN_POINT('Ctrl Pts',(0.0996491962474235,-0.0706287444932102,
-1.04083408558608E-17));
#17555=CARTESIAN_POINT('Ctrl Pts',(0.0938611946766418,-0.0771810981592459,
-1.06511292104842E-17));
#17556=CARTESIAN_POINT('Ctrl Pts',(0.0874218747326319,-0.0830961188460978,
9.460259835177E-18));
#17557=CARTESIAN_POINT('Ctrl Pts',(0.0803902102994179,-0.0882260767030795,
2.94902990916057E-17));
#17558=CARTESIAN_POINT('Ctrl Pts',(0.0765868618375105,-0.091000813397402,
4.03243227742548E-17));
#17559=CARTESIAN_POINT('Ctrl Pts',(0.0726097989303321,-0.0935451549285004,
-2.49510848448888E-18));
#17560=CARTESIAN_POINT('Ctrl Pts',(0.0684664424539416,-0.0958295198918429,
0.));
#17561=CARTESIAN_POINT('Ctrl Pts',(-0.00156962371674571,0.146072546381438,
1.50365));
#17562=CARTESIAN_POINT('Ctrl Pts',(0.0218361081466035,0.146362061217761,
1.50238307892777));
#17563=CARTESIAN_POINT('Ctrl Pts',(0.0452966847593804,0.141345883428421,
1.50111615785553));
#17564=CARTESIAN_POINT('Ctrl Pts',(0.0660179268768178,0.130913916311315,
1.4998492367833));
#17565=CARTESIAN_POINT('Ctrl Pts',(0.109300214423576,0.109123745727819,
1.4972029069042));
#17566=CARTESIAN_POINT('Ctrl Pts',(0.140630685714559,0.0637042888941242,
1.49455657702509));
#17567=CARTESIAN_POINT('Ctrl Pts',(0.145752650840527,0.0155206226173656,
1.49191024714599));
#17568=CARTESIAN_POINT('Ctrl Pts',(0.150874615966495,-0.0326630436593903,
1.48926391726689));
#17569=CARTESIAN_POINT('Ctrl Pts',(0.129788074927449,-0.0836109193792113,
1.48661758738779));
#17570=CARTESIAN_POINT('Ctrl Pts',(0.0921021927661857,-0.114042242015571,
1.48397125750869));
#17571=CARTESIAN_POINT('Ctrl Pts',(0.0544163106049216,-0.144473564651931,
1.48132492762959));
#17572=CARTESIAN_POINT('Ctrl Pts',(0.000131087321441313,-0.154388334204831,
1.47867859775048));
#17573=CARTESIAN_POINT('Ctrl Pts',(-0.0458840977328367,-0.139228052523514,
1.47603226787138));
#17574=CARTESIAN_POINT('Ctrl Pts',(-0.0918992827871148,-0.124067770842196,
1.47338593799228));
#17575=CARTESIAN_POINT('Ctrl Pts',(-0.129644429612189,-0.0838324379266627,
1.47073960811318));
#17576=CARTESIAN_POINT('Ctrl Pts',(-0.141854649713415,-0.0369491035797489,
1.46809327823408));
#17577=CARTESIAN_POINT('Ctrl Pts',(-0.14497337938942,-0.0249741805295802,
1.46741735368415));
#17578=CARTESIAN_POINT('Ctrl Pts',(-0.146426231435716,-0.0125655473306973,
1.46674142913422));
#17579=CARTESIAN_POINT('Ctrl Pts',(-0.14631473222987,-0.000131398079681141,
1.46606550458429));
#17580=CARTESIAN_POINT('Origin',(0.,0.,-0.0924367114736175));
#17581=CARTESIAN_POINT('',(-0.0684664424539507,-0.0958295198918364,0.));
#17582=CARTESIAN_POINT('Ctrl Pts',(-0.0686146973663072,-0.0959584553529141,
8.16675286424706E-17));
#17583=CARTESIAN_POINT('Ctrl Pts',(-0.0391968190522335,-0.116741470120209,
0.00244290680874874));
#17584=CARTESIAN_POINT('Ctrl Pts',(0.0436301113039178,-0.130476273073809,
0.0075332029917574));
#17585=CARTESIAN_POINT('Ctrl Pts',(0.134092250525203,-0.0374520209666004,
0.0152708885490261));
#17586=CARTESIAN_POINT('Ctrl Pts',(0.104134301645602,0.0924305194826295,
0.023213056671806));
#17587=CARTESIAN_POINT('Ctrl Pts',(-0.0212379681243542,0.137589894578696,
0.0311552247945861));
#17588=CARTESIAN_POINT('Ctrl Pts',(-0.106685947947232,0.0723488109778776,
0.0375631097285225));
#17589=CARTESIAN_POINT('Ctrl Pts',(-0.117663533972591,0.0165813593984342,
0.041323605288199));
#17590=CARTESIAN_POINT('Ctrl Pts',(-0.117600989619072,5.04992496179954E-5,
0.0424367114736154));
#17591=CARTESIAN_POINT('Origin',(0.,0.,0.));
#17592=CARTESIAN_POINT('Ctrl Pts',(-0.0510216505388318,0.106149619882943,
-0.0164977839420939));
#17593=CARTESIAN_POINT('Ctrl Pts',(-0.0863355867949722,0.0891756983861136,
-0.0138503945678339));
#17594=CARTESIAN_POINT('Ctrl Pts',(-0.13808023131828,0.0175094743621551,
-0.00855561581931395));
#17595=CARTESIAN_POINT('Ctrl Pts',(-0.0894531427980795,-0.106808298616542,
-0.000613447696533924));
#17596=CARTESIAN_POINT('Ctrl Pts',(0.0412394829729132,-0.132934609947913,
0.00732872042624606));
#17597=CARTESIAN_POINT('Ctrl Pts',(0.134092250525203,-0.0374520209666004,
0.0152708885490261));
#17598=CARTESIAN_POINT('Ctrl Pts',(0.104134301645602,0.0924305194826295,
0.023213056671806));
#17599=CARTESIAN_POINT('Ctrl Pts',(-0.0212379681243542,0.137589894578696,
0.0311552247945861));
#17600=CARTESIAN_POINT('Ctrl Pts',(-0.127145335141994,0.0567276974868182,
0.039097392917366));
#17601=CARTESIAN_POINT('Ctrl Pts',(-0.116579117211717,-0.0761160149501382,
0.0470395610401461));
#17602=CARTESIAN_POINT('Ctrl Pts',(0.000787973702835166,-0.139222729671589,
0.054981729162926));
#17603=CARTESIAN_POINT('Ctrl Pts',(0.117431922513572,-0.0747907597173192,
0.0629238972857061));
#17604=CARTESIAN_POINT('Ctrl Pts',(0.126496838785129,0.0581591461343325,
0.070866065408486));
#17605=CARTESIAN_POINT('Ctrl Pts',(0.0196773008918215,0.137828289815661,
0.0788082335312661));
#17606=CARTESIAN_POINT('Ctrl Pts',(-0.105168479521776,0.0912330920368172,
0.0867504016540459));
#17607=CARTESIAN_POINT('Ctrl Pts',(-0.133669226619255,-0.0389412707994331,
0.0946925697768262));
#17608=CARTESIAN_POINT('Ctrl Pts',(-0.0397151780004399,-0.133441281507892,
0.102634737899606));
#17609=CARTESIAN_POINT('Ctrl Pts',(0.0906220264938673,-0.105695447092796,
0.110576906022386));
#17610=CARTESIAN_POINT('Ctrl Pts',(0.137940159127448,0.0188783162799928,
0.118519074145166));
#17611=CARTESIAN_POINT('Ctrl Pts',(0.0588909273047484,0.126157580947307,
0.126461242267946));
#17612=CARTESIAN_POINT('Ctrl Pts',(-0.074108440039672,0.117863552156501,
0.134403410390726));
#17613=CARTESIAN_POINT('Ctrl Pts',(-0.139216864956951,0.00159439502933392,
0.142345578513506));
#17614=CARTESIAN_POINT('Ctrl Pts',(-0.0767883381764272,-0.116135388594389,
0.150287746636286));
#17615=CARTESIAN_POINT('Ctrl Pts',(0.0559861945572589,-0.127473226882309,
0.158229914759066));
#17616=CARTESIAN_POINT('Ctrl Pts',(0.137471621702818,-0.0220324926503626,
0.166172082881846));
#17617=CARTESIAN_POINT('Ctrl Pts',(0.0930189202108026,0.103592267873211,
0.174114251004626));
#17618=CARTESIAN_POINT('Ctrl Pts',(-0.0366486683060043,0.134315868829211,
0.182056419127406));
#17619=CARTESIAN_POINT('Ctrl Pts',(-0.132742311638566,0.0419923350165386,
0.189998587250186));
#17620=CARTESIAN_POINT('Ctrl Pts',(-0.107230360350792,-0.0888004916405464,
0.197940755372966));
#17621=CARTESIAN_POINT('Ctrl Pts',(0.0165156171993534,-0.138242945169174,
0.205882923495746));
#17622=CARTESIAN_POINT('Ctrl Pts',(0.125131592687617,-0.061040658666823,
0.213825091618526));
#17623=CARTESIAN_POINT('Ctrl Pts',(0.119114174013628,0.0720811421096423,
0.221767259741306));
#17624=CARTESIAN_POINT('Ctrl Pts',(0.0039759348809324,0.139169211541763,
0.229709427864086));
#17625=CARTESIAN_POINT('Ctrl Pts',(-0.114804669066963,0.0787639858025777,
0.237651595986866));
#17626=CARTESIAN_POINT('Ctrl Pts',(-0.128412401817242,-0.0537971426620367,
0.245593764109646));
#17627=CARTESIAN_POINT('Ctrl Pts',(-0.024381182195918,-0.137074561658528,
0.253535932232426));
#17628=CARTESIAN_POINT('Ctrl Pts',(0.101985705091022,-0.094777599970642,
0.261478100355206));
#17629=CARTESIAN_POINT('Ctrl Pts',(0.134923209124943,0.0343453801629359,
0.269420268477986));
#17630=CARTESIAN_POINT('Ctrl Pts',(0.0442571924125319,0.132004463632409,
0.277362436600766));
#17631=CARTESIAN_POINT('Ctrl Pts',(-0.0869529592639067,0.108733897080731,
0.285304604723546));
#17632=CARTESIAN_POINT('Ctrl Pts',(-0.138505267237684,-0.0141480898545381,
0.293246772846326));
#17633=CARTESIAN_POINT('Ctrl Pts',(-0.0631725212350128,-0.124068972994571,
0.301188940969106));
#17634=CARTESIAN_POINT('Ctrl Pts',(0.0700327441786229,-0.12032993078169,
0.309131109091886));
#17635=CARTESIAN_POINT('Ctrl Pts',(0.139080821187468,-0.00635631000930847,
0.317073277214666));
#17636=CARTESIAN_POINT('Ctrl Pts',(0.0807165776729536,0.11344034374014,
0.325015445337446));
#17637=CARTESIAN_POINT('Ctrl Pts',(-0.0515923433190751,0.129313988454311,
0.332957613460226));
#17638=CARTESIAN_POINT('Ctrl Pts',(-0.136637377548019,0.026722734813544,
0.340899781583006));
#17639=CARTESIAN_POINT('Ctrl Pts',(-0.0965085366518414,-0.100349289247285,
0.348841949705786));
#17640=CARTESIAN_POINT('Ctrl Pts',(0.0320320385160992,-0.135491055083419,
0.356784117828566));
#17641=CARTESIAN_POINT('Ctrl Pts',(0.131227975626944,-0.0465090949381858,
0.364726285951346));
#17642=CARTESIAN_POINT('Ctrl Pts',(0.110205605501345,0.0850799742312894,
0.372668454074126));
#17643=CARTESIAN_POINT('Ctrl Pts',(-0.0117764211155082,0.138727046407055,
0.380610622196906));
#17644=CARTESIAN_POINT('Ctrl Pts',(-0.122970036152848,0.065285892102983,
0.388552790319686));
#17645=CARTESIAN_POINT('Ctrl Pts',(-0.121510464882371,-0.0679638464419502,
0.396494958442466));
#17646=CARTESIAN_POINT('Ctrl Pts',(-0.00873482453528946,-0.138951719454826,
0.404437126565246));
#17647=CARTESIAN_POINT('Ctrl Pts',(0.112042812448737,-0.0826455423945668,
0.412379294688026));
#17648=CARTESIAN_POINT('Ctrl Pts',(0.130177722634257,0.049372441998279,
0.420321462810806));
#17649=CARTESIAN_POINT('Ctrl Pts',(0.0290564652212241,0.136160197297018,
0.428263630933586));
#17650=CARTESIAN_POINT('Ctrl Pts',(-0.098683499418539,0.098211223603141,
0.436205799056366));
#17651=CARTESIAN_POINT('Ctrl Pts',(-0.136019240449831,-0.0297093205335648,
0.444147967179146));
#17652=CARTESIAN_POINT('Ctrl Pts',(-0.0487473834415776,-0.130413074907061,
0.452090135301926));
#17653=CARTESIAN_POINT('Ctrl Pts',(0.0831820848081396,-0.111645054821459,
0.460032303424706));
#17654=CARTESIAN_POINT('Ctrl Pts',(0.138908217753341,0.00940130521287039,
0.467974471547486));
#17655=CARTESIAN_POINT('Ctrl Pts',(0.0673801526530663,0.121835103839429,
0.475916639670265));
#17656=CARTESIAN_POINT('Ctrl Pts',(-0.0658750545035054,0.12265543075329,
0.483858807793047));
#17657=CARTESIAN_POINT('Ctrl Pts',(-0.138781944133385,0.0111107822259715,
0.491800975915825));
#17658=CARTESIAN_POINT('Ctrl Pts',(-0.084550315326251,-0.110612484274364,
0.499743144038607));
#17659=CARTESIAN_POINT('Ctrl Pts',(0.0471380885036503,-0.131003351527116,
0.507685312161385));
#17660=CARTESIAN_POINT('Ctrl Pts',(0.135643160584381,-0.031381690295376,
0.515627480284167));
#17661=CARTESIAN_POINT('Ctrl Pts',(0.0998851624184703,0.0969888232104648,
0.523569648406945));
#17662=CARTESIAN_POINT('Ctrl Pts',(-0.0273779061153799,0.136507610615132,
0.531511816529727));
#17663=CARTESIAN_POINT('Ctrl Pts',(-0.129560000008381,0.0509714027366644,
0.539453984652505));
#17664=CARTESIAN_POINT('Ctrl Pts',(-0.113051823689188,-0.0812598465397498,
0.547396152775286));
#17665=CARTESIAN_POINT('Ctrl Pts',(0.00702343738442799,-0.139048728244533,
0.555338320898066));
#17666=CARTESIAN_POINT('Ctrl Pts',(0.12066450826877,-0.0694546898587181,
0.563280489020846));
#17667=CARTESIAN_POINT('Ctrl Pts',(0.123764493242992,0.063766979789076,
0.571222657143626));
#17668=CARTESIAN_POINT('Ctrl Pts',(0.0134834875971477,0.13857154491934,
0.579164825266405));
#17669=CARTESIAN_POINT('Ctrl Pts',(-0.109149777898995,0.0864303389077871,
0.587106993389186));
#17670=CARTESIAN_POINT('Ctrl Pts',(-0.131790633456927,-0.0448899368693808,
0.595049161511966));
#17671=CARTESIAN_POINT('Ctrl Pts',(-0.0336977294021144,-0.135086418755761,
0.602991329634746));
#17672=CARTESIAN_POINT('Ctrl Pts',(0.0952657566843092,-0.101529863106778,
0.610933497757526));
#17673=CARTESIAN_POINT('Ctrl Pts',(0.136956022624868,0.025038477707157,
0.618875665880307));
#17674=CARTESIAN_POINT('Ctrl Pts',(0.0531805018142573,0.128669000640787,
0.626817834003085));
#17675=CARTESIAN_POINT('Ctrl Pts',(-0.0793138220987445,0.114425500318782,
0.634760002125867));
#17676=CARTESIAN_POINT('Ctrl Pts',(-0.139148536750765,-0.00464351367351466,
0.642702170248646));
#17677=CARTESIAN_POINT('Ctrl Pts',(-0.0715088964667609,-0.119458592094588,
0.650644338371427));
#17678=CARTESIAN_POINT('Ctrl Pts',(0.0616402393688536,-0.124837327709565,
0.658586506494205));
#17679=CARTESIAN_POINT('Ctrl Pts',(0.138320583400205,-0.0158522461166236,
0.666528674616987));
#17680=CARTESIAN_POINT('Ctrl Pts',(0.0882850628235238,0.107655121482266,
0.674470842739765));
#17681=CARTESIAN_POINT('Ctrl Pts',(-0.0426286451686149,0.132539337972556,
0.682413010862546));
#17682=CARTESIAN_POINT('Ctrl Pts',(-0.13449013477919,0.0360039045964495,
0.690355178985326));
#17683=CARTESIAN_POINT('Ctrl Pts',(-0.103144844235522,-0.0935148042116587,
0.698297347108106));
#17684=CARTESIAN_POINT('Ctrl Pts',(0.022691720100341,-0.137364345221032,
0.706239515230886));
#17685=CARTESIAN_POINT('Ctrl Pts',(0.127740337615313,-0.0553740340325759,
0.714181683353665));
#17686=CARTESIAN_POINT('Ctrl Pts',(0.115765682611161,0.077344581120379,
0.722123851476446));
#17687=CARTESIAN_POINT('Ctrl Pts',(-0.00226223072526165,0.139207614056346,
0.730066019599226));
#17688=CARTESIAN_POINT('Ctrl Pts',(-0.118217708309552,0.0735421711751344,
0.738008187722006));
#17689=CARTESIAN_POINT('Ctrl Pts',(-0.125873620115675,-0.059495455776806,
0.745950355844786));
#17690=CARTESIAN_POINT('Ctrl Pts',(-0.0182163644075178,-0.138029133036789,
0.753892523967566));
#17691=CARTESIAN_POINT('Ctrl Pts',(0.106128952536144,-0.0901139441634624,
0.761834692090347));
#17692=CARTESIAN_POINT('Ctrl Pts',(0.133249245915149,0.0403548753208232,
0.769776860213125));
#17693=CARTESIAN_POINT('Ctrl Pts',(0.0382995408207276,0.133854483197375,
0.777719028335907));
#17694=CARTESIAN_POINT('Ctrl Pts',(-0.0917364783268051,0.104729633071593,
0.785661196458685));
#17695=CARTESIAN_POINT('Ctrl Pts',(-0.137732458880487,-0.0203383202317681,
0.793603364581467));
#17696=CARTESIAN_POINT('Ctrl Pts',(-0.0575513573065257,-0.126774282767806,
0.801545532704245));
#17697=CARTESIAN_POINT('Ctrl Pts',(0.0753527000357912,-0.117071978271622,
0.809487700827026));
#17698=CARTESIAN_POINT('Ctrl Pts',(0.139225942868322,-0.000119714417332432,
0.817429868949805));
#17699=CARTESIAN_POINT('Ctrl Pts',(0.0755539188089132,0.116942220141962,
0.825372037072586));
#17700=CARTESIAN_POINT('Ctrl Pts',(-0.0573332568284509,0.12687306712048,
0.833314205195366));
#17701=CARTESIAN_POINT('Ctrl Pts',(-0.13769727914169,0.0205751504512258,
0.841256373318145));
#17702=CARTESIAN_POINT('Ctrl Pts',(-0.0919164475821765,-0.104571717796869,
0.849198541440926));
#17703=CARTESIAN_POINT('Ctrl Pts',(0.0380692928980519,-0.133920149482284,
0.857140709563706));
#17704=CARTESIAN_POINT('Ctrl Pts',(0.133179650076608,-0.0405839661022353,
0.865082877686486));
#17705=CARTESIAN_POINT('Ctrl Pts',(0.106283765719693,0.0899312995767124,
0.873025045809266));
#17706=CARTESIAN_POINT('Ctrl Pts',(-0.0179789669825735,0.138060255849953,
0.880967213932046));
#17707=CARTESIAN_POINT('Ctrl Pts',(-0.125771118879347,0.0597118342956578,
0.888909382054826));
#17708=CARTESIAN_POINT('Ctrl Pts',(-0.118344004924669,-0.0733387619032726,
0.896851550177606));
#17709=CARTESIAN_POINT('Ctrl Pts',(-0.00250162451743248,-0.139203517821528,
0.904793718300386));
#17710=CARTESIAN_POINT('Ctrl Pts',(0.115632500949424,-0.0775435504945224,
0.912735886423165));
#17711=CARTESIAN_POINT('Ctrl Pts',(0.127835376168433,0.0551542754370876,
0.920678054545947));
#17712=CARTESIAN_POINT('Ctrl Pts',(0.0229279137899797,0.137325118854324,
0.928620222668725));
#17713=CARTESIAN_POINT('Ctrl Pts',(-0.102983873094174,0.0936920454555137,
0.936562390791507));
#17714=CARTESIAN_POINT('Ctrl Pts',(-0.134551852288801,-0.0357725669300891,
0.944504558914285));
#17715=CARTESIAN_POINT('Ctrl Pts',(-0.0428565117498991,-0.132465832952297,
0.952446727037066));
#17716=CARTESIAN_POINT('Ctrl Pts',(0.0880997963686447,-0.107806787258123,
0.960388895159846));
#17717=CARTESIAN_POINT('Ctrl Pts',(0.138347640177547,0.0156143509765511,
0.968331063282625));
#17718=CARTESIAN_POINT('Ctrl Pts',(0.061854832590724,0.124731139593481,
0.976273231405407));
#17719=CARTESIAN_POINT('Ctrl Pts',(-0.0713033562375951,0.119581390225944,
0.984215399528185));
#17720=CARTESIAN_POINT('Ctrl Pts',(-0.139140345480169,0.00488280234845834,
0.992157567650966));
#17721=CARTESIAN_POINT('Ctrl Pts',(-0.0795104838321055,-0.114288934109561,
1.00009973577375));
#17722=CARTESIAN_POINT('Ctrl Pts',(0.0529591494285269,-0.128760265574912,
1.00804190389653));
#17723=CARTESIAN_POINT('Ctrl Pts',(0.136912761112491,-0.0252739657289669,
1.0159840720193));
#17724=CARTESIAN_POINT('Ctrl Pts',(0.0954402180350474,0.101365883217864,
1.02392624014209));
#17725=CARTESIAN_POINT('Ctrl Pts',(-0.0334653697086341,0.135144169424284,
1.03186840826486));
#17726=CARTESIAN_POINT('Ctrl Pts',(-0.131713240771149,0.0451165125500212,
1.03981057638765));
#17727=CARTESIAN_POINT('Ctrl Pts',(-0.109298251871946,-0.0862425048155002,
1.04775274451043));
#17728=CARTESIAN_POINT('Ctrl Pts',(0.0132451643780021,-0.13859452774087,
1.05569491263321));
#17729=CARTESIAN_POINT('Ctrl Pts',(0.123654649330263,-0.0639797248987874,
1.06363708075599));
#17730=CARTESIAN_POINT('Ctrl Pts',(0.120783771971213,0.0692470788374567,
1.07157924887876));
#17731=CARTESIAN_POINT('Ctrl Pts',(0.00726255089817806,0.139036444335888,
1.07952141700155));
#17732=CARTESIAN_POINT('Ctrl Pts',(-0.112911912907791,0.0814541430660127,
1.08746358512433));
#17733=CARTESIAN_POINT('Ctrl Pts',(-0.129647464608677,-0.0507485213543897,
1.09540575324711));
#17734=CARTESIAN_POINT('Ctrl Pts',(-0.0276126195379174,-0.136460326620484,
1.10334792136989));
#17735=CARTESIAN_POINT('Ctrl Pts',(0.0997182217817603,-0.0971604536002107,
1.11129008949267));
#17736=CARTESIAN_POINT('Ctrl Pts',(0.135696927507188,0.0311483765905046,
1.11923225761545));
#17737=CARTESIAN_POINT('Ctrl Pts',(0.0473633069609982,0.130922093830007,
1.12717442573822));
#17738=CARTESIAN_POINT('Ctrl Pts',(-0.0843599685788644,0.110757722983492,
1.13511659386101));
#17739=CARTESIAN_POINT('Ctrl Pts',(-0.138800846271631,-0.0108721006891078,
1.14305876198379));
#17740=CARTESIAN_POINT('Ctrl Pts',(-0.0660858892268601,-0.122541963197144,
1.15100093010657));
#17741=CARTESIAN_POINT('Ctrl Pts',(0.0671705316110708,-0.121950798202395,
1.15894309822935));
#17742=CARTESIAN_POINT('Ctrl Pts',(0.138891844802359,-0.00964017357273747,
1.16688526635212));
#17743=CARTESIAN_POINT('Ctrl Pts',(0.0833739592533277,0.111501840422208,
1.17482743447491));
#17744=CARTESIAN_POINT('Ctrl Pts',(-0.0485230383040216,0.130496713571114,
1.18276960259768));
#17745=CARTESIAN_POINT('Ctrl Pts',(-0.135967947813762,0.0299431906521225,
1.19071177072047));
#17746=CARTESIAN_POINT('Ctrl Pts',(-0.0988522486080867,-0.0980413710850678,
1.19865393884324));
#17747=CARTESIAN_POINT('Ctrl Pts',(0.0288222657999454,-0.136209964735594,
1.20659610696603));
#17748=CARTESIAN_POINT('Ctrl Pts',(0.130092623711363,-0.0495962373069701,
1.21453827508881));
#17749=CARTESIAN_POINT('Ctrl Pts',(0.112184773380136,0.082452738709893,
1.22248044321158));
#17750=CARTESIAN_POINT('Ctrl Pts',(-0.00849585454694533,0.138966535376798,
1.23042261133437));
#17751=CARTESIAN_POINT('Ctrl Pts',(-0.121393406896754,0.0681727090639588,
1.23836477945715));
#17752=CARTESIAN_POINT('Ctrl Pts',(-0.123082127310551,-0.0650743223999996,
1.24630694757992));
#17753=CARTESIAN_POINT('Ctrl Pts',(-0.0120149744006178,-0.138706589206355,
1.25424911570271));
#17754=CARTESIAN_POINT('Ctrl Pts',(0.110059129405696,-0.0852693704304675,
1.26219128382548));
#17755=CARTESIAN_POINT('Ctrl Pts',(0.13130776387206,0.0462833517151888,
1.27013345194827));
#17756=CARTESIAN_POINT('Ctrl Pts',(0.0322649968732001,0.135435768819968,
1.27807562007105));
#17757=CARTESIAN_POINT('Ctrl Pts',(-0.0963358219719167,0.100515107841202,
1.28601778819382));
#17758=CARTESIAN_POINT('Ctrl Pts',(-0.136683130933199,-0.0264877182308561,
1.29395995631661));
#17759=CARTESIAN_POINT('Ctrl Pts',(-0.0518146499729274,-0.129225073214149,
1.30190212443939));
#17760=CARTESIAN_POINT('Ctrl Pts',(0.0805213734929343,-0.11357898534207,
1.30984429256217));
#17761=CARTESIAN_POINT('Ctrl Pts',(0.1390915465469,0.0061171215252809,1.31778646068495));
#17762=CARTESIAN_POINT('Ctrl Pts',(0.0702395735793815,0.120209316621791,
1.32572862880773));
#17763=CARTESIAN_POINT('Ctrl Pts',(-0.0629590648350173,0.124177428154433,
1.33367079693051));
#17764=CARTESIAN_POINT('Ctrl Pts',(-0.138480731711197,0.0143862582011507,
1.34161296505328));
#17765=CARTESIAN_POINT('Ctrl Pts',(-0.0871398218994898,-0.108584202098263,
1.34955513317607));
#17766=CARTESIAN_POINT('Ctrl Pts',(0.0440301174146577,-0.132080378229483,
1.35749730129884));
#17767=CARTESIAN_POINT('Ctrl Pts',(0.13486394497766,-0.0345773583278084,
1.36543946942163));
#17768=CARTESIAN_POINT('Ctrl Pts',(0.102148545386143,0.0946020732301706,
1.3733816375444));
#17769=CARTESIAN_POINT('Ctrl Pts',(-0.0241454188302812,0.137116288461919,
1.38132380566719));
#17770=CARTESIAN_POINT('Ctrl Pts',(-0.128319693277533,0.0540178939468163,
1.38926597378996));
#17771=CARTESIAN_POINT('Ctrl Pts',(-0.114939956470138,-0.0785664351508689,
1.39720814191275));
#17772=CARTESIAN_POINT('Ctrl Pts',(0.00373660876362508,-0.139175849115243,
1.40515031003553));
#17773=CARTESIAN_POINT('Ctrl Pts',(0.118990018389619,-0.0722858665142316,
1.41309247815831));
#17774=CARTESIAN_POINT('Ctrl Pts',(0.125236419206141,0.0608253567263532,
1.42103464628109));
#17775=CARTESIAN_POINT('Ctrl Pts',(0.0167532566496359,0.13821437898841,
1.42897681440387));
#17776=CARTESIAN_POINT('Ctrl Pts',(-0.107077349343502,0.0889846891406984,
1.43691898252665));
#17777=CARTESIAN_POINT('Ctrl Pts',(-0.132814597987359,-0.0417638487589672,
1.44486115064943));
#17778=CARTESIAN_POINT('Ctrl Pts',(-0.0368790902657646,-0.134252921254984,
1.45280331877221));
#17779=CARTESIAN_POINT('Ctrl Pts',(0.0928396680879532,-0.103751556080299,
1.46074548689499));
#17780=CARTESIAN_POINT('Ctrl Pts',(0.137511141307062,0.0217950526079239,
1.46868765501776));
#17781=CARTESIAN_POINT('Ctrl Pts',(0.0562018483347667,0.127378648737854,
1.47662982314055));
#17782=CARTESIAN_POINT('Ctrl Pts',(-0.0765818961642769,0.116263681173923,
1.48457199126332));
#17783=CARTESIAN_POINT('Ctrl Pts',(-0.13923195096087,-0.00134816270381636,
1.49251415938611));
#17784=CARTESIAN_POINT('Ctrl Pts',(-0.0742871760264013,-0.117748889605885,
1.50045632750888));
#17785=CARTESIAN_POINT('Ctrl Pts',(0.0586284551779338,-0.126233948370975,
1.50839849563167));
#17786=CARTESIAN_POINT('Ctrl Pts',(0.137995068118234,-0.019163470063063,
1.51634066375444));
#17787=CARTESIAN_POINT('Ctrl Pts',(0.0906261803825392,0.105639137646141,
1.52428283187723));
#17788=CARTESIAN_POINT('Ctrl Pts',(0.00417072711528833,0.124051375507138,
1.52957761062575));
#17789=CARTESIAN_POINT('Ctrl Pts',(-0.0334019664627544,0.1129391839063,
1.53222500000001));
#17790=CARTESIAN_POINT('Ctrl Pts',(-0.0551480035117261,0.114734422509858,
-0.0109985226280628));
#17791=CARTESIAN_POINT('Ctrl Pts',(-0.093317938433455,0.0963877427684319,
-0.00835113325380276));
#17792=CARTESIAN_POINT('Ctrl Pts',(-0.149247407742026,0.0189255452031589,
-0.00305635450528277));
#17793=CARTESIAN_POINT('Ctrl Pts',(-0.0966876253720675,-0.115446371588928,
0.00488581361749726));
#17794=CARTESIAN_POINT('Ctrl Pts',(0.0445747075563756,-0.143685636564375,
0.0128279817402772));
#17795=CARTESIAN_POINT('Ctrl Pts',(0.144936900801175,-0.0404809362687151,
0.0207701498630572));
#17796=CARTESIAN_POINT('Ctrl Pts',(0.112556116319125,0.0999057960529736,
0.0287123179858373));
#17797=CARTESIAN_POINT('Ctrl Pts',(-0.0229555792165621,0.148717415239805,
0.0366544861086172));
#17798=CARTESIAN_POINT('Ctrl Pts',(-0.137428156769908,0.0613155244327884,
0.0445966542313972));
#17799=CARTESIAN_POINT('Ctrl Pts',(-0.126007400730642,-0.0822718633254329,
0.0525388223541772));
#17800=CARTESIAN_POINT('Ctrl Pts',(0.000851700720621877,-0.150482305134309,
0.0604809904769572));
#17801=CARTESIAN_POINT('Ctrl Pts',(0.126929176276611,-0.0808394286734405,
0.0684231585997372));
#17802=CARTESIAN_POINT('Ctrl Pts',(0.136727213562698,0.0628627408439891,
0.0763653267225173));
#17803=CARTESIAN_POINT('Ctrl Pts',(0.0212686937255662,0.148975090584026,
0.0843074948452972));
#17804=CARTESIAN_POINT('Ctrl Pts',(-0.113673932864549,0.0986115272026031,
0.0922496629680772));
#17805=CARTESIAN_POINT('Ctrl Pts',(-0.144479665027646,-0.0420906285100245,
0.100191831090857));
#17806=CARTESIAN_POINT('Ctrl Pts',(-0.0429271251068198,-0.144233284958223,
0.108133999213637));
#17807=CARTESIAN_POINT('Ctrl Pts',(0.0979510420095061,-0.114243518700172,
0.116076167336417));
#17808=CARTESIAN_POINT('Ctrl Pts',(0.149096007275942,0.0204050915936607,
0.124018335459197));
#17809=CARTESIAN_POINT('Ctrl Pts',(0.0636537044864716,0.136360518400275,
0.131960503581977));
#17810=CARTESIAN_POINT('Ctrl Pts',(-0.0801019266996435,0.127395713772213,
0.139902671704757));
#17811=CARTESIAN_POINT('Ctrl Pts',(-0.15047596611352,0.00172334100814176,
0.147844839827537));
#17812=CARTESIAN_POINT('Ctrl Pts',(-0.0829985603893774,-0.125527785761544,
0.155787007950317));
#17813=CARTESIAN_POINT('Ctrl Pts',(0.0605140527882773,-0.137782566606816,
0.163729176073097));
#17814=CARTESIAN_POINT('Ctrl Pts',(0.148589577098441,-0.0238143605552183,
0.171671344195877));
#17815=CARTESIAN_POINT('Ctrl Pts',(0.100541783424623,0.111970245809892,
0.179613512318657));
#17816=CARTESIAN_POINT('Ctrl Pts',(-0.0396126128240685,0.145178604134651,
0.187555680441437));
#17817=CARTESIAN_POINT('Ctrl Pts',(-0.143477786216001,0.0453884461694337,
0.195497848564217));
#17818=CARTESIAN_POINT('Ctrl Pts',(-0.115902567375552,-0.095982191346566,
0.203440016686997));
#17819=CARTESIAN_POINT('Ctrl Pts',(0.0178513102906219,-0.149423281002214,
0.211382184809777));
#17820=CARTESIAN_POINT('Ctrl Pts',(0.135251553802876,-0.0659772944027704,
0.219324352932557));
#17821=CARTESIAN_POINT('Ctrl Pts',(0.128747479107914,0.07791067196398,0.227266521055337));
#17822=CARTESIAN_POINT('Ctrl Pts',(0.00429748682099232,0.150424458749874,
0.235208689178117));
#17823=CARTESIAN_POINT('Ctrl Pts',(-0.124089444892588,0.0851339876261335,
0.243150857300897));
#17824=CARTESIAN_POINT('Ctrl Pts',(-0.138797696890977,-0.0581479623084488,
0.251093025423677));
#17825=CARTESIAN_POINT('Ctrl Pts',(-0.0263529993083425,-0.148160405002171,
0.259035193546457));
#17826=CARTESIAN_POINT('Ctrl Pts',(0.110233752987369,-0.102442695616748,
0.266977361669237));
#17827=CARTESIAN_POINT('Ctrl Pts',(0.145835062802846,0.0371230472913779,
0.274919529792017));
#17828=CARTESIAN_POINT('Ctrl Pts',(0.0478364728857143,0.142680265085169,
0.282861697914797));
#17829=CARTESIAN_POINT('Ctrl Pts',(-0.0939852406223356,0.117527701960322,
0.290803866037577));
#17830=CARTESIAN_POINT('Ctrl Pts',(-0.14970681824969,-0.01529231023972,
0.298746034160357));
#17831=CARTESIAN_POINT('Ctrl Pts',(-0.0682815703945392,-0.134102995221473,
0.306688202283137));
#17832=CARTESIAN_POINT('Ctrl Pts',(0.0756966107742644,-0.1300615596562,
0.314630370405917));
#17833=CARTESIAN_POINT('Ctrl Pts',(0.150328919865546,-0.00687037371415525,
0.322572538528697));
#17834=CARTESIAN_POINT('Ctrl Pts',(0.0872444944832666,0.122614780370367,
0.330514706651477));
#17835=CARTESIAN_POINT('Ctrl Pts',(-0.0557648508131485,0.139772198940638,
0.338456874774257));
#17836=CARTESIAN_POINT('Ctrl Pts',(-0.147687863823926,0.0288839239377102,
0.346399042897038));
#17837=CARTESIAN_POINT('Ctrl Pts',(-0.104313621021262,-0.10846499275041,
0.354341211019817));
#17838=CARTESIAN_POINT('Ctrl Pts',(0.0346226151823369,-0.146448833047075,
0.362283379142597));
#17839=CARTESIAN_POINT('Ctrl Pts',(0.141840978962514,-0.0502704970123603,
0.370225547265377));
#17840=CARTESIAN_POINT('Ctrl Pts',(0.119118434135606,0.0919607787700563,
0.378167715388157));
#17841=CARTESIAN_POINT('Ctrl Pts',(-0.0127288338612142,0.149946533709345,
0.386109883510937));
#17842=CARTESIAN_POINT('Ctrl Pts',(-0.132915182358376,0.070565859178174,
0.394052051633717));
#17843=CARTESIAN_POINT('Ctrl Pts',(-0.131337568919768,-0.0734603918663599,
0.401994219756497));
#17844=CARTESIAN_POINT('Ctrl Pts',(-0.00944124952954395,-0.150189377088511,
0.409936387879277));
#17845=CARTESIAN_POINT('Ctrl Pts',(0.121104224366159,-0.0893294633566384,
0.417878556002057));
#17846=CARTESIAN_POINT('Ctrl Pts',(0.140705787232781,0.0533654159743681,
0.425820724124838));
#17847=CARTESIAN_POINT('Ctrl Pts',(0.0314063937394313,0.147172091835368,
0.433762892247617));
#17848=CARTESIAN_POINT('Ctrl Pts',(-0.106664482920656,0.106154012011714,
0.441705060370398));
#17849=CARTESIAN_POINT('Ctrl Pts',(-0.147019735166745,-0.032112048430678,
0.449647228493177));
#17850=CARTESIAN_POINT('Ctrl Pts',(-0.052689806088835,-0.14096017351449,
0.457589396615958));
#17851=CARTESIAN_POINT('Ctrl Pts',(0.0899093983958942,-0.120674298270189,
0.465531564738737));
#17852=CARTESIAN_POINT('Ctrl Pts',(0.15014235720654,0.0101616315312987,
0.473473732861518));
#17853=CARTESIAN_POINT('Ctrl Pts',(0.0728294921055832,0.131688462906045,
0.481415900984297));
#17854=CARTESIAN_POINT('Ctrl Pts',(-0.071202669822089,0.132575133389036,
0.489358069107078));
#17855=CARTESIAN_POINT('Ctrl Pts',(-0.150005871264529,0.012009361726732,
0.497300237229857));
#17856=CARTESIAN_POINT('Ctrl Pts',(-0.0913882839399832,-0.119558219045865,
0.505242405352637));
#17857=CARTESIAN_POINT('Ctrl Pts',(0.0509503601487159,-0.141598188489932,
0.513184573475417));
#17858=CARTESIAN_POINT('Ctrl Pts',(0.146613240011817,-0.0339196703426114,
0.521126741598197));
#17859=CARTESIAN_POINT('Ctrl Pts',(0.107963329873666,0.104832750538675,
0.529068909720978));
#17860=CARTESIAN_POINT('Ctrl Pts',(-0.0295920819230583,0.147547602048875,
0.537011077843756));
#17861=CARTESIAN_POINT('Ctrl Pts',(-0.140038106568177,0.055093691941219,
0.544953245966537));
#17862=CARTESIAN_POINT('Ctrl Pts',(-0.122194838935542,-0.0878316999746162,
0.552895414089317));
#17863=CARTESIAN_POINT('Ctrl Pts',(0.00759145471482065,-0.150294231420327,
0.560837582212097));
#17864=CARTESIAN_POINT('Ctrl Pts',(0.130423195946632,-0.0750718065719766,
0.568779750334878));
#17865=CARTESIAN_POINT('Ctrl Pts',(0.133773890807325,0.0689241055160235,
0.576721918457657));
#17866=CARTESIAN_POINT('Ctrl Pts',(0.0145739585745413,0.149778456108953,
0.584664086580438));
#17867=CARTESIAN_POINT('Ctrl Pts',(-0.117977216952174,0.0934203535806499,
0.592606254703216));
#17868=CARTESIAN_POINT('Ctrl Pts',(-0.142449141490696,-0.0485203902651028,
0.600548422825998));
#17869=CARTESIAN_POINT('Ctrl Pts',(-0.036423018067407,-0.146011471938939,
0.608490590948776));
#17870=CARTESIAN_POINT('Ctrl Pts',(0.102970331784443,-0.109741044988262,
0.616432759071558));
#17871=CARTESIAN_POINT('Ctrl Pts',(0.148032279177632,0.0270634532975707,
0.624374927194337));
#17872=CARTESIAN_POINT('Ctrl Pts',(0.0574814509102497,0.139075048028633,
0.632317095317117));
#17873=CARTESIAN_POINT('Ctrl Pts',(-0.0857282916847416,0.123679611042927,
0.640259263439898));
#17874=CARTESIAN_POINT('Ctrl Pts',(-0.150402111894479,-0.00501905574730406,
0.648201431562677));
#17875=CARTESIAN_POINT('Ctrl Pts',(-0.0772921462128499,-0.129119751845818,
0.656143599685457));
#17876=CARTESIAN_POINT('Ctrl Pts',(0.0666253659236285,-0.134933490277457,
0.664085767808237));
#17877=CARTESIAN_POINT('Ctrl Pts',(0.14950719819016,-0.0171342893707992,
0.672027935931017));
#17878=CARTESIAN_POINT('Ctrl Pts',(0.0954250774564579,0.11636168087194,
0.679970104053797));
#17879=CARTESIAN_POINT('Ctrl Pts',(-0.0460762176180427,0.143258397146306,
0.687912272176577));
#17880=CARTESIAN_POINT('Ctrl Pts',(-0.145366963764729,0.0389157041403328,
0.695854440299358));
#17881=CARTESIAN_POINT('Ctrl Pts',(-0.111486636987321,-0.101077771820372,
0.703796608422136));
#17882=CARTESIAN_POINT('Ctrl Pts',(0.02452690272786,-0.148473624679578,
0.711738776544918));
#17883=CARTESIAN_POINT('Ctrl Pts',(0.138071279799868,-0.0598523840572839,
0.719680944667696));
#17884=CARTESIAN_POINT('Ctrl Pts',(0.125128179973684,0.0835997892305201,
0.727623112790477));
#17885=CARTESIAN_POINT('Ctrl Pts',(-0.00244518761474098,0.150465967050502,
0.735565280913257));
#17886=CARTESIAN_POINT('Ctrl Pts',(-0.127778512144395,0.0794898610961098,
0.743507449036036));
#17887=CARTESIAN_POINT('Ctrl Pts',(-0.136053592364468,-0.0643071239260258,
0.751449617158818));
#17888=CARTESIAN_POINT('Ctrl Pts',(-0.019689604662082,-0.149192176910068,
0.759391785281597));
#17889=CARTESIAN_POINT('Ctrl Pts',(0.114712083700712,-0.0974018687498071,
0.767333953404378));
#17890=CARTESIAN_POINT('Ctrl Pts',(0.144025718573537,0.0436185576594447,
0.775276121527157));
#17891=CARTESIAN_POINT('Ctrl Pts',(0.0413969989087525,0.14467990414796,
0.783218289649938));
#17892=CARTESIAN_POINT('Ctrl Pts',(-0.0991556246317344,0.113199594905656,
0.791160457772717));
#17893=CARTESIAN_POINT('Ctrl Pts',(-0.148871509365196,-0.021983172706469,
0.799102625895497));
#17894=CARTESIAN_POINT('Ctrl Pts',(-0.062205797368885,-0.137027095702329,
0.807044794018277));
#17895=CARTESIAN_POINT('Ctrl Pts',(0.081446815661698,-0.126540121706451,
0.814986962141057));
#17896=CARTESIAN_POINT('Ctrl Pts',(0.150485778196879,-0.000129396266831759,
0.822929130263837));
#17897=CARTESIAN_POINT('Ctrl Pts',(0.0816643079123276,0.126399869446589,
0.830871298386618));
#17898=CARTESIAN_POINT('Ctrl Pts',(-0.0619700581130299,0.137133869194964,
0.838813466509397));
#17899=CARTESIAN_POINT('Ctrl Pts',(-0.148833484480893,0.0222391564630926,
0.846755634632177));
#17900=CARTESIAN_POINT('Ctrl Pts',(-0.0993501488194509,-0.113028908304323,
0.854697802754957));
#17901=CARTESIAN_POINT('Ctrl Pts',(0.041148129789194,-0.144750881164039,
0.862639970877736));
#17902=CARTESIAN_POINT('Ctrl Pts',(0.143950494202948,-0.0438661760544617,
0.870582139000517));
#17903=CARTESIAN_POINT('Ctrl Pts',(0.114879417330645,0.0972044528644933,
0.878524307123298));
#17904=CARTESIAN_POINT('Ctrl Pts',(-0.0194330078274841,0.149225816766708,
0.886466475246077));
#17905=CARTESIAN_POINT('Ctrl Pts',(-0.135942801386891,0.0645410019599824,
0.894408643368857));
#17906=CARTESIAN_POINT('Ctrl Pts',(-0.127915022941288,-0.0792700011911429,
0.902350811491637));
#17907=CARTESIAN_POINT('Ctrl Pts',(-0.00270394227186439,-0.150461539534541,
0.910292979614417));
#17908=CARTESIAN_POINT('Ctrl Pts',(0.124984227305131,-0.0838148501630433,
0.918235147737197));
#17909=CARTESIAN_POINT('Ctrl Pts',(0.138174004553101,0.0596148525845174,
0.926177315859977));
#17910=CARTESIAN_POINT('Ctrl Pts',(0.0247821984756025,0.148431225898158,
0.934119483982757));
#17911=CARTESIAN_POINT('Ctrl Pts',(-0.11131264737753,0.101269347369872,
0.942061652105537));
#17912=CARTESIAN_POINT('Ctrl Pts',(-0.145433672650089,-0.0386656571445607,
0.950003820228317));
#17913=CARTESIAN_POINT('Ctrl Pts',(-0.0463225128062989,-0.143178947440692,
0.957945988351097));
#17914=CARTESIAN_POINT('Ctrl Pts',(0.0952248276606132,-0.116525612549003,
0.965888156473877));
#17915=CARTESIAN_POINT('Ctrl Pts',(0.149536443172165,0.0168771545685866,
0.973830324596656));
#17916=CARTESIAN_POINT('Ctrl Pts',(0.0668573142755158,0.134818714245386,
0.981772492719438));
#17917=CARTESIAN_POINT('Ctrl Pts',(-0.0770699830103684,0.129252481220654,
0.989714660842216));
#17918=CARTESIAN_POINT('Ctrl Pts',(-0.15039325815857,0.00527769678589187,
0.997656828964997));
#17919=CARTESIAN_POINT('Ctrl Pts',(-0.0859408583470751,-0.123532000103139,
1.00559899708778));
#17920=CARTESIAN_POINT('Ctrl Pts',(0.0572421967501742,-0.139173693973137,
1.01354116521056));
#17921=CARTESIAN_POINT('Ctrl Pts',(0.147985518909957,-0.0273179863069172,
1.02148333333334));
#17922=CARTESIAN_POINT('Ctrl Pts',(0.103158902618224,0.109563803299803,
1.02942550145612));
#17923=CARTESIAN_POINT('Ctrl Pts',(-0.0361718663885326,0.146073893166727,
1.0373676695789));
#17924=CARTESIAN_POINT('Ctrl Pts',(-0.142365489706367,0.0487652901517079,
1.04530983770168));
#17925=CARTESIAN_POINT('Ctrl Pts',(-0.118137698690712,-0.0932173284908804,
1.05325200582446));
#17926=CARTESIAN_POINT('Ctrl Pts',(0.0143163610725534,-0.149803297655807,
1.06119417394724));
#17927=CARTESIAN_POINT('Ctrl Pts',(0.133655163317704,-0.0691540562905145,
1.06913634207002));
#17928=CARTESIAN_POINT('Ctrl Pts',(0.130552105047211,0.0748474051030229,
1.0770785101928));
#17929=CARTESIAN_POINT('Ctrl Pts',(0.0078499064261323,0.150280954056111,
1.08502067831558));
#17930=CARTESIAN_POINT('Ctrl Pts',(-0.122043612932812,0.0880417101447944,
1.09296284643836));
#17931=CARTESIAN_POINT('Ctrl Pts',(-0.140132644828567,-0.0548527851276936,
1.10090501456114));
#17932=CARTESIAN_POINT('Ctrl Pts',(-0.0298457776877653,-0.147496493982489,
1.10884718268392));
#17933=CARTESIAN_POINT('Ctrl Pts',(0.107782887988268,-0.10501826145877,
1.1167893508067));
#17934=CARTESIAN_POINT('Ctrl Pts',(0.146671355310253,0.033667487497105,
1.12473151892948));
#17935=CARTESIAN_POINT('Ctrl Pts',(0.0511937930472066,0.141510359113225,
1.13267368705226));
#17936=CARTESIAN_POINT('Ctrl Pts',(-0.0911825429852659,0.119715203870077,
1.14061585517504));
#17937=CARTESIAN_POINT('Ctrl Pts',(-0.150026302104679,-0.0117513769282424,
1.14855802329782));
#17938=CARTESIAN_POINT('Ctrl Pts',(-0.0714305557085884,-0.132452489195471,
1.1565001914206));
#17939=CARTESIAN_POINT('Ctrl Pts',(0.0726029180563751,-0.131813513998426,
1.16444235954338));
#17940=CARTESIAN_POINT('Ctrl Pts',(0.150124660100533,-0.010419818262018,
1.17238452766616));
#17941=CARTESIAN_POINT('Ctrl Pts',(0.0901167906002831,0.120519501471002,
1.18032669578894));
#17942=CARTESIAN_POINT('Ctrl Pts',(-0.0524473171394798,0.141050576417769,
1.18826886391172));
#17943=CARTESIAN_POINT('Ctrl Pts',(-0.146964294261872,0.0323648326895764,
1.1962110320345));
#17944=CARTESIAN_POINT('Ctrl Pts',(-0.106846879624786,-0.105970422747861,
1.20415320015727));
#17945=CARTESIAN_POINT('Ctrl Pts',(0.0311532535456026,-0.14722588419309,
1.21209536828006));
#17946=CARTESIAN_POINT('Ctrl Pts',(0.140613805972886,-0.0536073106276968,
1.22003753640283));
#17947=CARTESIAN_POINT('Ctrl Pts',(0.121257666323848,0.0891210667609394,
1.22797970452562));
#17948=CARTESIAN_POINT('Ctrl Pts',(-0.00918295295119051,0.150205391241489,
1.2359218726484));
#17949=CARTESIAN_POINT('Ctrl Pts',(-0.131211043922368,0.0736861461587066,
1.24386404077118));
#17950=CARTESIAN_POINT('Ctrl Pts',(-0.133036338837895,-0.0703371788708997,
1.25180620889396));
#17951=CARTESIAN_POINT('Ctrl Pts',(-0.0129866800356469,-0.149924422041766,
1.25974837701674));
#17952=CARTESIAN_POINT('Ctrl Pts',(0.118960111851797,-0.0921654923014072,
1.26769054513952));
#17953=CARTESIAN_POINT('Ctrl Pts',(0.141927220045961,0.050026496908035,
1.2756327132623));
#17954=CARTESIAN_POINT('Ctrl Pts',(0.0348744139414821,0.146389075532006,
1.28357488138508));
#17955=CARTESIAN_POINT('Ctrl Pts',(-0.104126938119509,0.108644221848311,
1.29151704950786));
#17956=CARTESIAN_POINT('Ctrl Pts',(-0.147737317493493,-0.0286299004949125,
1.29945921763064));
#17957=CARTESIAN_POINT('Ctrl Pts',(-0.0560051364173496,-0.139676092720537,
1.30740138575342));
#17958=CARTESIAN_POINT('Ctrl Pts',(0.0870335032532438,-0.122764634549313,
1.3153435538762));
#17959=CARTESIAN_POINT('Ctrl Pts',(0.150340512633584,0.00661184096937889,
1.32328572199898));
#17960=CARTESIAN_POINT('Ctrl Pts',(0.0759201674095095,0.129931190880528,
1.33122789012176));
#17961=CARTESIAN_POINT('Ctrl Pts',(-0.0680508508044829,0.134220221643466,
1.33917005824454));
#17962=CARTESIAN_POINT('Ctrl Pts',(-0.149680298423566,0.0155497403439283,
1.34711222636732));
#17963=CARTESIAN_POINT('Ctrl Pts',(-0.0941872156892785,-0.117365900463673,
1.3550543944901));
#17964=CARTESIAN_POINT('Ctrl Pts',(0.0475910332998192,-0.142762319241037,
1.36299656261288));
#17965=CARTESIAN_POINT('Ctrl Pts',(0.145771005694385,-0.0373737865856905,
1.37093873073566));
#17966=CARTESIAN_POINT('Ctrl Pts',(0.110409762917901,0.10225297323032,1.37888089885844));
#17967=CARTESIAN_POINT('Ctrl Pts',(-0.0260981686868614,0.148205506441964,
1.38682306698121));
#17968=CARTESIAN_POINT('Ctrl Pts',(-0.138697490589939,0.0583865667538053,
1.394765235104));
#17969=CARTESIAN_POINT('Ctrl Pts',(-0.124235673603468,-0.0849204601545819,
1.40270740322677));
#17970=CARTESIAN_POINT('Ctrl Pts',(0.0040388053119065,-0.150431633134115,
1.41064957134956));
#17971=CARTESIAN_POINT('Ctrl Pts',(0.12861328245382,-0.0781319533624403,
1.41859173947234));
#17972=CARTESIAN_POINT('Ctrl Pts',(0.1353648581188,0.0657445800149866,1.42653390759512));
#17973=CARTESIAN_POINT('Ctrl Pts',(0.0181081687242482,0.149392404544468,
1.43447607571789));
#17974=CARTESIAN_POINT('Ctrl Pts',(-0.115737181672069,0.0961812857364522,
1.44241824384068));
#17975=CARTESIAN_POINT('Ctrl Pts',(-0.143555918690644,-0.0451414811888502,
1.45036041196346));
#17976=CARTESIAN_POINT('Ctrl Pts',(-0.0398616700558823,-0.145110565703753,
1.45830258008624));
#17977=CARTESIAN_POINT('Ctrl Pts',(0.100348034367198,-0.112142416378873,
1.46624474820902));
#17978=CARTESIAN_POINT('Ctrl Pts',(0.14863229283285,0.0235577176564554,
1.4741869163318));
#17979=CARTESIAN_POINT('Ctrl Pts',(0.0607471474677608,0.137680339497592,
1.48212908445458));
#17980=CARTESIAN_POINT('Ctrl Pts',(-0.0827754224726193,0.125666453945577,
1.49007125257736));
#17981=CARTESIAN_POINT('Ctrl Pts',(-0.150492272191201,-0.00145719475437189,
1.49801342070014));
#17982=CARTESIAN_POINT('Ctrl Pts',(-0.0802951178786721,-0.12727177793954,
1.50595558882292));
#17983=CARTESIAN_POINT('Ctrl Pts',(0.0633700050447994,-0.136443062004882,
1.5138977569457));
#17984=CARTESIAN_POINT('Ctrl Pts',(0.149155357006591,-0.0207133070603065,
1.52183992506848));
#17985=CARTESIAN_POINT('Ctrl Pts',(0.0979555318420461,0.114182655252422,
1.52978209319126));
#17986=CARTESIAN_POINT('Ctrl Pts',(0.00450803278943675,0.134083974545181,
1.53507687193978));
#17987=CARTESIAN_POINT('Ctrl Pts',(-0.0361033354337414,0.122073089461022,
1.53772426131404));
#17988=CARTESIAN_POINT('Ctrl Pts',(-0.0592743564846203,0.123319225136773,
-0.00549926131403157));
#17989=CARTESIAN_POINT('Ctrl Pts',(-0.100300290071938,0.10359978715075,
-0.00285187193977157));
#17990=CARTESIAN_POINT('Ctrl Pts',(-0.160414584165772,0.0203416160441626,
0.00244290680874841));
#17991=CARTESIAN_POINT('Ctrl Pts',(-0.103922107946056,-0.124084444561314,
0.0103850749315284));
#17992=CARTESIAN_POINT('Ctrl Pts',(0.0479099321398382,-0.154436663180837,
0.0183272430543084));
#17993=CARTESIAN_POINT('Ctrl Pts',(0.155781551077148,-0.0435098515708298,
0.0262694111770884));
#17994=CARTESIAN_POINT('Ctrl Pts',(0.120977930992648,0.107381072623318,
0.0342115792998684));
#17995=CARTESIAN_POINT('Ctrl Pts',(-0.0246731903087699,0.159844935900913,
0.0421537474226484));
#17996=CARTESIAN_POINT('Ctrl Pts',(-0.147710978397823,0.0659033513787588,
0.0500959155454284));
#17997=CARTESIAN_POINT('Ctrl Pts',(-0.135435684249567,-0.0884277117007276,
0.0580380836682085));
#17998=CARTESIAN_POINT('Ctrl Pts',(0.000915427738408385,-0.16174188059703,
0.0659802517909884));
#17999=CARTESIAN_POINT('Ctrl Pts',(0.13642643003965,-0.0868880976295618,
0.0739224199137684));
#18000=CARTESIAN_POINT('Ctrl Pts',(0.146957588340267,0.0675663355536457,
0.0818645880365484));
#18001=CARTESIAN_POINT('Ctrl Pts',(0.0228600865593111,0.160121891352391,
0.0898067561593285));
#18002=CARTESIAN_POINT('Ctrl Pts',(-0.122179386207322,0.105989962368389,
0.0977489242821083));
#18003=CARTESIAN_POINT('Ctrl Pts',(-0.155290103436038,-0.0452399862206161,
0.105691092404888));
#18004=CARTESIAN_POINT('Ctrl Pts',(-0.0461390722131997,-0.155025288408554,
0.113633260527668));
#18005=CARTESIAN_POINT('Ctrl Pts',(0.105280057525145,-0.122791590307548,
0.121575428650448));
#18006=CARTESIAN_POINT('Ctrl Pts',(0.160251855424436,0.0219318669073289,
0.129517596773229));
#18007=CARTESIAN_POINT('Ctrl Pts',(0.0684164816681947,0.146563455853242,
0.137459764896008));
#18008=CARTESIAN_POINT('Ctrl Pts',(-0.086095413359615,0.136927875387926,
0.145401933018789));
#18009=CARTESIAN_POINT('Ctrl Pts',(-0.16173506727009,0.00185228698694943,
0.153344101141568));
#18010=CARTESIAN_POINT('Ctrl Pts',(-0.0892087826023274,-0.134920182928699,
0.161286269264348));
#18011=CARTESIAN_POINT('Ctrl Pts',(0.0650419110192955,-0.148091906331324,
0.169228437387128));
#18012=CARTESIAN_POINT('Ctrl Pts',(0.159707532494063,-0.025596228460074,
0.177170605509908));
#18013=CARTESIAN_POINT('Ctrl Pts',(0.108064646638443,0.120348223746572,
0.185112773632688));
#18014=CARTESIAN_POINT('Ctrl Pts',(-0.0425765573421325,0.156041339440091,
0.193054941755468));
#18015=CARTESIAN_POINT('Ctrl Pts',(-0.154213260793436,0.0487845573223287,
0.200997109878248));
#18016=CARTESIAN_POINT('Ctrl Pts',(-0.124574774400312,-0.103163891052585,
0.208939278001028));
#18017=CARTESIAN_POINT('Ctrl Pts',(0.0191870033818907,-0.160603616835255,
0.216881446123808));
#18018=CARTESIAN_POINT('Ctrl Pts',(0.145371514918136,-0.0709139301387177,
0.224823614246588));
#18019=CARTESIAN_POINT('Ctrl Pts',(0.138380784202201,0.0837402018183176,
0.232765782369368));
#18020=CARTESIAN_POINT('Ctrl Pts',(0.00461903876105218,0.161679705957985,
0.240707950492149));
#18021=CARTESIAN_POINT('Ctrl Pts',(-0.133374220718213,0.0915039894496894,
0.248650118614928));
#18022=CARTESIAN_POINT('Ctrl Pts',(-0.149182991964712,-0.0624987819548612,
0.256592286737709));
#18023=CARTESIAN_POINT('Ctrl Pts',(-0.0283248164207669,-0.159246248345813,
0.264534454860488));
#18024=CARTESIAN_POINT('Ctrl Pts',(0.118481800883715,-0.110107791262854,
0.272476622983269));
#18025=CARTESIAN_POINT('Ctrl Pts',(0.156746916480749,0.0399007144198201,
0.280418791106048));
#18026=CARTESIAN_POINT('Ctrl Pts',(0.0514157533588968,0.153356066537929,
0.288360959228829));
#18027=CARTESIAN_POINT('Ctrl Pts',(-0.101017521980764,0.126321506839912,
0.296303127351608));
#18028=CARTESIAN_POINT('Ctrl Pts',(-0.160908369261695,-0.0164365306249019,
0.304245295474388));
#18029=CARTESIAN_POINT('Ctrl Pts',(-0.0733906195540655,-0.144137017448375,
0.312187463597168));
#18030=CARTESIAN_POINT('Ctrl Pts',(0.0813604773699057,-0.13979318853071,
0.320129631719948));
#18031=CARTESIAN_POINT('Ctrl Pts',(0.161577018543625,-0.00738443741900211,
0.328071799842729));
#18032=CARTESIAN_POINT('Ctrl Pts',(0.0937724112935796,0.131789217000595,
0.336013967965508));
#18033=CARTESIAN_POINT('Ctrl Pts',(-0.0599373583072218,0.150230409426965,
0.343956136088289));
#18034=CARTESIAN_POINT('Ctrl Pts',(-0.158738350099833,0.0310451130618767,
0.351898304211068));
#18035=CARTESIAN_POINT('Ctrl Pts',(-0.112118705390683,-0.116580696253536,
0.359840472333849));
#18036=CARTESIAN_POINT('Ctrl Pts',(0.0372131918485748,-0.15740661101073,
0.367782640456628));
#18037=CARTESIAN_POINT('Ctrl Pts',(0.152453982298084,-0.0540318990865351,
0.375724808579408));
#18038=CARTESIAN_POINT('Ctrl Pts',(0.128031262769868,0.0988415833088236,
0.383666976702188));
#18039=CARTESIAN_POINT('Ctrl Pts',(-0.0136812466069205,0.161166021011634,
0.391609144824968));
#18040=CARTESIAN_POINT('Ctrl Pts',(-0.142860328563903,0.0758458262533652,
0.399551312947749));
#18041=CARTESIAN_POINT('Ctrl Pts',(-0.141164672957165,-0.0789569372907697,
0.407493481070528));
#18042=CARTESIAN_POINT('Ctrl Pts',(-0.0101476745237983,-0.161427034722196,
0.415435649193308));
#18043=CARTESIAN_POINT('Ctrl Pts',(0.130165636283581,-0.0960133843187101,
0.423377817316089));
#18044=CARTESIAN_POINT('Ctrl Pts',(0.151233851831306,0.0573583899504574,
0.431319985438868));
#18045=CARTESIAN_POINT('Ctrl Pts',(0.0337563222576384,0.158183986373718,
0.439262153561649));
#18046=CARTESIAN_POINT('Ctrl Pts',(-0.114645466422773,0.114096800420287,
0.447204321684428));
#18047=CARTESIAN_POINT('Ctrl Pts',(-0.158020229883659,-0.0345147763277912,
0.455146489807208));
#18048=CARTESIAN_POINT('Ctrl Pts',(-0.0566322287360923,-0.151507272121918,
0.463088657929988));
#18049=CARTESIAN_POINT('Ctrl Pts',(0.0966367119836487,-0.129703541718919,
0.471030826052768));
#18050=CARTESIAN_POINT('Ctrl Pts',(0.161376496659739,0.0109219578497271,
0.478972994175549));
#18051=CARTESIAN_POINT('Ctrl Pts',(0.0782788315581001,0.141541821972661,
0.486915162298328));
#18052=CARTESIAN_POINT('Ctrl Pts',(-0.0765302851406724,0.142494836024782,
0.494857330421108));
#18053=CARTESIAN_POINT('Ctrl Pts',(-0.161229798395673,0.0129079412274925,
0.502799498543889));
#18054=CARTESIAN_POINT('Ctrl Pts',(-0.0982262525537151,-0.128503953817366,
0.510741666666668));
#18055=CARTESIAN_POINT('Ctrl Pts',(0.0547626317937811,-0.152193025452748,
0.518683834789449));
#18056=CARTESIAN_POINT('Ctrl Pts',(0.157583319439253,-0.0364576503898468,
0.526626002912228));
#18057=CARTESIAN_POINT('Ctrl Pts',(0.116041497328862,0.112676677866884,
0.534568171035008));
#18058=CARTESIAN_POINT('Ctrl Pts',(-0.0318062577307366,0.158587593482618,
0.542510339157789));
#18059=CARTESIAN_POINT('Ctrl Pts',(-0.150516213127973,0.0592159811457737,
0.550452507280567));
#18060=CARTESIAN_POINT('Ctrl Pts',(-0.131337854181896,-0.0944035534094825,
0.558394675403349));
#18061=CARTESIAN_POINT('Ctrl Pts',(0.00815947204521347,-0.161539734596121,
0.566336843526128));
#18062=CARTESIAN_POINT('Ctrl Pts',(0.140181883624494,-0.080688923285235,
0.574279011648909));
#18063=CARTESIAN_POINT('Ctrl Pts',(0.143783288371658,0.0740812312429708,
0.582221179771688));
#18064=CARTESIAN_POINT('Ctrl Pts',(0.0156644295519346,0.160985367298567,
0.590163347894469));
#18065=CARTESIAN_POINT('Ctrl Pts',(-0.126804656005353,0.100410368253513,
0.598105516017247));
#18066=CARTESIAN_POINT('Ctrl Pts',(-0.153107649524464,-0.0521508436608248,
0.606047684140029));
#18067=CARTESIAN_POINT('Ctrl Pts',(-0.0391483067326994,-0.156936525122116,
0.613989852262808));
#18068=CARTESIAN_POINT('Ctrl Pts',(0.110674906884577,-0.117952226869747,
0.621932020385589));
#18069=CARTESIAN_POINT('Ctrl Pts',(0.159108535730396,0.0290884288879846,
0.629874188508368));
#18070=CARTESIAN_POINT('Ctrl Pts',(0.061782400006242,0.14948109541648,0.637816356631148));
#18071=CARTESIAN_POINT('Ctrl Pts',(-0.0921427612707386,0.132933721767072,
0.645758524753929));
#18072=CARTESIAN_POINT('Ctrl Pts',(-0.161655687038194,-0.0053945978210935,
0.653700692876707));
#18073=CARTESIAN_POINT('Ctrl Pts',(-0.0830753959589387,-0.138780911597048,
0.661642860999489));
#18074=CARTESIAN_POINT('Ctrl Pts',(0.0716104924784035,-0.145029652845349,
0.669585029122267));
#18075=CARTESIAN_POINT('Ctrl Pts',(0.160693812980115,-0.0184163326249747,
0.677527197245049));
#18076=CARTESIAN_POINT('Ctrl Pts',(0.102565092089392,0.125068240261613,
0.685469365367828));
#18077=CARTESIAN_POINT('Ctrl Pts',(-0.0495237900674707,0.153977456320057,
0.693411533490608));
#18078=CARTESIAN_POINT('Ctrl Pts',(-0.156243792750268,0.0418275036842162,
0.701353701613389));
#18079=CARTESIAN_POINT('Ctrl Pts',(-0.119828429739121,-0.108640739429086,
0.709295869736167));
#18080=CARTESIAN_POINT('Ctrl Pts',(0.0263620853553792,-0.159582904138124,
0.717238037858949));
#18081=CARTESIAN_POINT('Ctrl Pts',(0.148402221984423,-0.0643307340819919,
0.725180205981728));
#18082=CARTESIAN_POINT('Ctrl Pts',(0.134490677336207,0.0898549973406614,
0.733122374104509));
#18083=CARTESIAN_POINT('Ctrl Pts',(-0.00262814450422035,0.161724320044658,
0.741064542227287));
#18084=CARTESIAN_POINT('Ctrl Pts',(-0.137339315979238,0.0854375510170853,
0.749006710350069));
#18085=CARTESIAN_POINT('Ctrl Pts',(-0.146233564613262,-0.0691187920752458,
0.756948878472847));
#18086=CARTESIAN_POINT('Ctrl Pts',(-0.0211628449166461,-0.160355220783347,
0.764891046595629));
#18087=CARTESIAN_POINT('Ctrl Pts',(0.12329521486528,-0.104689793336152,
0.772833214718408));
#18088=CARTESIAN_POINT('Ctrl Pts',(0.154802191231926,0.0468822399980663,
0.780775382841188));
#18089=CARTESIAN_POINT('Ctrl Pts',(0.0444944569967772,0.155505325098544,
0.788717550963968));
#18090=CARTESIAN_POINT('Ctrl Pts',(-0.106574770936664,0.121669556739719,
0.796659719086747));
#18091=CARTESIAN_POINT('Ctrl Pts',(-0.160010559849905,-0.0236280251811701,
0.804601887209529));
#18092=CARTESIAN_POINT('Ctrl Pts',(-0.0668602374312443,-0.147279908636853,
0.812544055332307));
#18093=CARTESIAN_POINT('Ctrl Pts',(0.0875409312876049,-0.13600826514128,
0.820486223455089));
#18094=CARTESIAN_POINT('Ctrl Pts',(0.161745613525436,-0.000139078116330951,
0.828428391577867));
#18095=CARTESIAN_POINT('Ctrl Pts',(0.0877746970157421,0.135857518751215,
0.836370559700649));
#18096=CARTESIAN_POINT('Ctrl Pts',(-0.0666068593976089,0.147394671269449,
0.844312727823428));
#18097=CARTESIAN_POINT('Ctrl Pts',(-0.159969689820096,0.0239031624749592,
0.852254895946208));
#18098=CARTESIAN_POINT('Ctrl Pts',(-0.106783850056725,-0.121486098811777,
0.860197064068988));
#18099=CARTESIAN_POINT('Ctrl Pts',(0.0442269666803361,-0.155581612845794,
0.868139232191768));
#18100=CARTESIAN_POINT('Ctrl Pts',(0.154721338329289,-0.0471483860066884,
0.876081400314548));
#18101=CARTESIAN_POINT('Ctrl Pts',(0.123475068941597,0.104477606152275,
0.884023568437328));
#18102=CARTESIAN_POINT('Ctrl Pts',(-0.0208870486723946,0.160391377683462,
0.891965736560109));
#18103=CARTESIAN_POINT('Ctrl Pts',(-0.146114483894434,0.0693701696243073,
0.899907904682887));
#18104=CARTESIAN_POINT('Ctrl Pts',(-0.137486040957907,-0.0852012404790134,
0.907850072805669));
#18105=CARTESIAN_POINT('Ctrl Pts',(-0.00290626002629624,-0.161719561247554,
0.915792240928448));
#18106=CARTESIAN_POINT('Ctrl Pts',(0.134335953660838,-0.0900861498315643,
0.923734409051229));
#18107=CARTESIAN_POINT('Ctrl Pts',(0.148512632937768,0.0640754297319473,
0.931676577174007));
#18108=CARTESIAN_POINT('Ctrl Pts',(0.0266364831612253,0.159537332941991,
0.939618745296788));
#18109=CARTESIAN_POINT('Ctrl Pts',(-0.119641421660886,0.10884664928423,
0.947560913419568));
#18110=CARTESIAN_POINT('Ctrl Pts',(-0.156315493011378,-0.0415587473590326,
0.955503081542348));
#18111=CARTESIAN_POINT('Ctrl Pts',(-0.0497885138626987,-0.153892061929087,
0.963445249665127));
#18112=CARTESIAN_POINT('Ctrl Pts',(0.102349858952582,-0.125244437839883,
0.971387417787908));
#18113=CARTESIAN_POINT('Ctrl Pts',(0.160725246166783,0.018139958160622,
0.979329585910688));
#18114=CARTESIAN_POINT('Ctrl Pts',(0.0718597959603077,0.14490628889729,
0.987271754033468));
#18115=CARTESIAN_POINT('Ctrl Pts',(-0.0828366097831417,0.138923572215364,
0.995213922156248));
#18116=CARTESIAN_POINT('Ctrl Pts',(-0.161646170836971,0.00567259122332548,
1.00315609027903));
#18117=CARTESIAN_POINT('Ctrl Pts',(-0.0923712328620446,-0.132775066096718,
1.01109825840181));
#18118=CARTESIAN_POINT('Ctrl Pts',(0.0615252440718216,-0.149587122371362,
1.01904042652459));
#18119=CARTESIAN_POINT('Ctrl Pts',(0.159058276707423,-0.0293620068848675,
1.02698259464737));
#18120=CARTESIAN_POINT('Ctrl Pts',(0.1108775872014,0.117761723381742,1.03492476277015));
#18121=CARTESIAN_POINT('Ctrl Pts',(-0.0388783630684312,0.157003616909169,
1.04286693089293));
#18122=CARTESIAN_POINT('Ctrl Pts',(-0.153017738641585,0.0524140677533946,
1.05080909901571));
#18123=CARTESIAN_POINT('Ctrl Pts',(-0.126977145509477,-0.10019215216626,
1.05875126713849));
#18124=CARTESIAN_POINT('Ctrl Pts',(0.0153875577671049,-0.161012067570745,
1.06669343526127));
#18125=CARTESIAN_POINT('Ctrl Pts',(0.143655677305146,-0.0743283876822416,
1.07463560338405));
#18126=CARTESIAN_POINT('Ctrl Pts',(0.140320438123209,0.080447731368589,
1.08257777150683));
#18127=CARTESIAN_POINT('Ctrl Pts',(0.00843726195408678,0.161525463776335,
1.09051993962961));
#18128=CARTESIAN_POINT('Ctrl Pts',(-0.131175312957834,0.094629277223576,
1.09846210775239));
#18129=CARTESIAN_POINT('Ctrl Pts',(-0.150617825048456,-0.0589570489009974,
1.10640427587517));
#18130=CARTESIAN_POINT('Ctrl Pts',(-0.0320789358376135,-0.158532661344495,
1.11434644399795));
#18131=CARTESIAN_POINT('Ctrl Pts',(0.115847554194776,-0.112876069317329,
1.12228861212073));
#18132=CARTESIAN_POINT('Ctrl Pts',(0.157645783113317,0.0361865984037055,
1.13023078024351));
#18133=CARTESIAN_POINT('Ctrl Pts',(0.0550242791334153,0.152098624396442,
1.13817294836629));
#18134=CARTESIAN_POINT('Ctrl Pts',(-0.0980051173916675,0.128672684756662,
1.14611511648907));
#18135=CARTESIAN_POINT('Ctrl Pts',(-0.161251757937727,-0.0126306531673768,
1.15405728461185));
#18136=CARTESIAN_POINT('Ctrl Pts',(-0.0767752221903169,-0.142363015193798,
1.16199945273463));
#18137=CARTESIAN_POINT('Ctrl Pts',(0.0780353045016797,-0.141676229794458,
1.16994162085741));
#18138=CARTESIAN_POINT('Ctrl Pts',(0.161357475398708,-0.0111994629512984,
1.17788378898019));
#18139=CARTESIAN_POINT('Ctrl Pts',(0.0968596219472387,0.129537162519796,
1.18582595710297));
#18140=CARTESIAN_POINT('Ctrl Pts',(-0.0563715959749383,0.151604439264423,
1.19376812522575));
#18141=CARTESIAN_POINT('Ctrl Pts',(-0.157960640709981,0.0347864747270306,
1.20171029334853));
#18142=CARTESIAN_POINT('Ctrl Pts',(-0.114841510641486,-0.113899474410655,
1.20965246147131));
#18143=CARTESIAN_POINT('Ctrl Pts',(0.03348424129126,-0.158241803650584,
1.21759462959409));
#18144=CARTESIAN_POINT('Ctrl Pts',(0.151134988234409,-0.0576183839484237,
1.22553679771687));
#18145=CARTESIAN_POINT('Ctrl Pts',(0.130330559267559,0.0957893948119858,
1.23347896583965));
#18146=CARTESIAN_POINT('Ctrl Pts',(-0.0098700513554357,0.16144424710618,
1.24142113396243));
#18147=CARTESIAN_POINT('Ctrl Pts',(-0.141028680947982,0.0791995832534545,
1.24936330208521));
#18148=CARTESIAN_POINT('Ctrl Pts',(-0.142990550365238,-0.0756000353418,
1.25730547020799));
#18149=CARTESIAN_POINT('Ctrl Pts',(-0.013958385670676,-0.161142254877177,
1.26524763833077));
#18150=CARTESIAN_POINT('Ctrl Pts',(0.127861094297897,-0.0990616141723472,
1.27318980645355));
#18151=CARTESIAN_POINT('Ctrl Pts',(0.152546676219863,0.0537696421008814,
1.28113197457633));
#18152=CARTESIAN_POINT('Ctrl Pts',(0.0374838310097642,0.157342382244044,
1.28907414269911));
#18153=CARTESIAN_POINT('Ctrl Pts',(-0.111918054267102,0.116773335855419,
1.29701631082189));
#18154=CARTESIAN_POINT('Ctrl Pts',(-0.158791504053787,-0.0307720827589687,
1.30495847894467));
#18155=CARTESIAN_POINT('Ctrl Pts',(-0.060195622861772,-0.150127112226926,
1.31290064706745));
#18156=CARTESIAN_POINT('Ctrl Pts',(0.0935456330135535,-0.131950283756556,
1.32084281519023));
#18157=CARTESIAN_POINT('Ctrl Pts',(0.161589478720268,0.00710656041347678,
1.32878498331301));
#18158=CARTESIAN_POINT('Ctrl Pts',(0.0816007612396376,0.139653065139265,
1.33672715143579));
#18159=CARTESIAN_POINT('Ctrl Pts',(-0.0731426367739486,0.144263015132499,
1.34466931955857));
#18160=CARTESIAN_POINT('Ctrl Pts',(-0.160879865135934,0.0167132224867059,
1.35261148768135));
#18161=CARTESIAN_POINT('Ctrl Pts',(-0.101234609479067,-0.126147598829082,
1.36055365580413));
#18162=CARTESIAN_POINT('Ctrl Pts',(0.051151949184981,-0.153444260252591,
1.36849582392691));
#18163=CARTESIAN_POINT('Ctrl Pts',(0.15667806641111,-0.0401702148435725,
1.37643799204969));
#18164=CARTESIAN_POINT('Ctrl Pts',(0.118670980449659,0.10990387323047,1.38438016017247));
#18165=CARTESIAN_POINT('Ctrl Pts',(-0.0280509185434417,0.159294724422008,
1.39232232829525));
#18166=CARTESIAN_POINT('Ctrl Pts',(-0.149075287902345,0.0627552395607943,
1.40026449641803));
#18167=CARTESIAN_POINT('Ctrl Pts',(-0.133531390736797,-0.0912744851582948,
1.40820666454081));
#18168=CARTESIAN_POINT('Ctrl Pts',(0.00434100186018791,-0.161687417152987,
1.41614883266359));
#18169=CARTESIAN_POINT('Ctrl Pts',(0.138236546518021,-0.0839780402106489,
1.42409100078637));
#18170=CARTESIAN_POINT('Ctrl Pts',(0.145493297031458,0.07066380330362,1.43203316890915));
#18171=CARTESIAN_POINT('Ctrl Pts',(0.0194630807988606,0.160570430100525,
1.43997533703193));
#18172=CARTESIAN_POINT('Ctrl Pts',(-0.124397014000637,0.103377882332206,
1.44791750515471));
#18173=CARTESIAN_POINT('Ctrl Pts',(-0.15429723939393,-0.0485191136187331,
1.45585967327749));
#18174=CARTESIAN_POINT('Ctrl Pts',(-0.042844249846,-0.155968210152522,1.46380184140027));
#18175=CARTESIAN_POINT('Ctrl Pts',(0.107856400646442,-0.120533276677448,
1.47174400952305));
#18176=CARTESIAN_POINT('Ctrl Pts',(0.159753444358638,0.0253203827049868,
1.47968617764583));
#18177=CARTESIAN_POINT('Ctrl Pts',(0.0652924466007548,0.147982030257331,
1.48762834576861));
#18178=CARTESIAN_POINT('Ctrl Pts',(-0.0889689487809616,0.13506922671723,
1.49557051389139));
#18179=CARTESIAN_POINT('Ctrl Pts',(-0.161752593421533,-0.00156622680492735,
1.50351268201417));
#18180=CARTESIAN_POINT('Ctrl Pts',(-0.086303059730943,-0.136794666273195,
1.51145485013695));
#18181=CARTESIAN_POINT('Ctrl Pts',(0.0681115549116652,-0.14665217563879,
1.51939701825973));
#18182=CARTESIAN_POINT('Ctrl Pts',(0.160315645894948,-0.02226314405755,
1.52733918638251));
#18183=CARTESIAN_POINT('Ctrl Pts',(0.105284883301553,0.122726172858702,
1.53528135450529));
#18184=CARTESIAN_POINT('Ctrl Pts',(0.00484533846358528,0.144116573583224,
1.54057613325381));
#18185=CARTESIAN_POINT('Ctrl Pts',(-0.0388047044047284,0.131206995015745,
1.54322352262807));
#18186=CARTESIAN_POINT('Ctrl Pts',(-0.0634007094575145,0.131904027763688,
-3.88578058618805E-16));
#18187=CARTESIAN_POINT('Ctrl Pts',(-0.107282641710421,0.110811831533068,
0.00264738937425961));
#18188=CARTESIAN_POINT('Ctrl Pts',(-0.171581760589518,0.0217576868851663,
0.0079421681227796));
#18189=CARTESIAN_POINT('Ctrl Pts',(-0.111156590520044,-0.1327225175337,
0.0158843362455596));
#18190=CARTESIAN_POINT('Ctrl Pts',(0.0512451567233008,-0.165187689797298,
0.0238265043683396));
#18191=CARTESIAN_POINT('Ctrl Pts',(0.16662620135312,-0.0465387668729445,
0.0317686724911196));
#18192=CARTESIAN_POINT('Ctrl Pts',(0.129399745666171,0.114856349193662,
0.0397108406138996));
#18193=CARTESIAN_POINT('Ctrl Pts',(-0.026390801400978,0.170972456562021,
0.0476530087366796));
#18194=CARTESIAN_POINT('Ctrl Pts',(-0.157993800025737,0.070491178324729,
0.0555951768594596));
#18195=CARTESIAN_POINT('Ctrl Pts',(-0.144863967768493,-0.0945835600760224,
0.0635373449822396));
#18196=CARTESIAN_POINT('Ctrl Pts',(0.000979154756195248,-0.17300145605975,
0.0714795131050195));
#18197=CARTESIAN_POINT('Ctrl Pts',(0.145923683802689,-0.0929367665856833,
0.0794216812277997));
#18198=CARTESIAN_POINT('Ctrl Pts',(0.157187963117837,0.0722699302633024,
0.0873638493505794));
#18199=CARTESIAN_POINT('Ctrl Pts',(0.0244514793930555,0.171268692120756,
0.0953060174733598));
#18200=CARTESIAN_POINT('Ctrl Pts',(-0.130684839550095,0.113368397534175,
0.103248185596139));
#18201=CARTESIAN_POINT('Ctrl Pts',(-0.166100541844429,-0.0483893439312075,
0.11119035371892));
#18202=CARTESIAN_POINT('Ctrl Pts',(-0.0493510193195793,-0.165817291858885,
0.119132521841699));
#18203=CARTESIAN_POINT('Ctrl Pts',(0.112609073040783,-0.131339661914923,
0.12707468996448));
#18204=CARTESIAN_POINT('Ctrl Pts',(0.17140770357293,0.0234586422209967,
0.135016858087259));
#18205=CARTESIAN_POINT('Ctrl Pts',(0.0731792588499177,0.156766393306209,
0.14295902621004));
#18206=CARTESIAN_POINT('Ctrl Pts',(-0.0920889000195865,0.146460037003638,
0.150901194332819));
#18207=CARTESIAN_POINT('Ctrl Pts',(-0.172994168426659,0.00198123296575728,
0.1588433624556));
#18208=CARTESIAN_POINT('Ctrl Pts',(-0.0954190048152776,-0.144312580095855,
0.16678553057838));
#18209=CARTESIAN_POINT('Ctrl Pts',(0.0695697692503139,-0.158401246055831,
0.17472769870116));
#18210=CARTESIAN_POINT('Ctrl Pts',(0.170825487889685,-0.0273780963649298,
0.18266986682394));
#18211=CARTESIAN_POINT('Ctrl Pts',(0.115587509852263,0.128726201683253,
0.19061203494672));
#18212=CARTESIAN_POINT('Ctrl Pts',(-0.0455405018601966,0.16690407474553,
0.198554203069499));
#18213=CARTESIAN_POINT('Ctrl Pts',(-0.164948735370872,0.0521806684752238,
0.20649637119228));
#18214=CARTESIAN_POINT('Ctrl Pts',(-0.133246981425072,-0.110345590758605,
0.214438539315059));
#18215=CARTESIAN_POINT('Ctrl Pts',(0.0205226964731592,-0.171783952668295,
0.22238070743784));
#18216=CARTESIAN_POINT('Ctrl Pts',(0.155491476033395,-0.0758505658746651,
0.230322875560619));
#18217=CARTESIAN_POINT('Ctrl Pts',(0.148014089296488,0.0895697316726553,
0.2382650436834));
#18218=CARTESIAN_POINT('Ctrl Pts',(0.00494059070111224,0.172934953166096,
0.24620721180618));
#18219=CARTESIAN_POINT('Ctrl Pts',(-0.142658996543838,0.0978739912732451,
0.25414937992896));
#18220=CARTESIAN_POINT('Ctrl Pts',(-0.159568287038446,-0.0668496016012732,
0.262091548051739));
#18221=CARTESIAN_POINT('Ctrl Pts',(-0.0302966335331915,-0.170332091689456,
0.27003371617452));
#18222=CARTESIAN_POINT('Ctrl Pts',(0.126729848780061,-0.11777288690896,
0.2779758842973));
#18223=CARTESIAN_POINT('Ctrl Pts',(0.167658770158652,0.0426783815482623,
0.28591805242008));
#18224=CARTESIAN_POINT('Ctrl Pts',(0.0549950338320791,0.164031867990689,
0.293860220542859));
#18225=CARTESIAN_POINT('Ctrl Pts',(-0.108049803339193,0.135115311719503,
0.30180238866564));
#18226=CARTESIAN_POINT('Ctrl Pts',(-0.1721099202737,-0.0175807510100837,
0.309744556788419));
#18227=CARTESIAN_POINT('Ctrl Pts',(-0.0784996687135917,-0.154171039675278,
0.3176867249112));
#18228=CARTESIAN_POINT('Ctrl Pts',(0.087024343965547,-0.14952481740522,
0.325628893033979));
#18229=CARTESIAN_POINT('Ctrl Pts',(0.172825117221703,-0.00789850112384905,
0.33357106115676));
#18230=CARTESIAN_POINT('Ctrl Pts',(0.100300328103893,0.140963653630822,
0.341513229279539));
#18231=CARTESIAN_POINT('Ctrl Pts',(-0.0641098658012952,0.160688619913292,
0.349455397402319));
#18232=CARTESIAN_POINT('Ctrl Pts',(-0.16978883637574,0.033206302186043,
0.357397565525099));
#18233=CARTESIAN_POINT('Ctrl Pts',(-0.119923789760104,-0.124696399756661,
0.36533973364788));
#18234=CARTESIAN_POINT('Ctrl Pts',(0.0398037685148125,-0.168364388974385,
0.373281901770659));
#18235=CARTESIAN_POINT('Ctrl Pts',(0.163066985633654,-0.0577933011607096,
0.38122406989344));
#18236=CARTESIAN_POINT('Ctrl Pts',(0.136944091404129,0.10572238784759,0.38916623801622));
#18237=CARTESIAN_POINT('Ctrl Pts',(-0.0146336593526265,0.172385508313924,
0.397108406138999));
#18238=CARTESIAN_POINT('Ctrl Pts',(-0.152805474769431,0.0811257933285562,
0.40505057426178));
#18239=CARTESIAN_POINT('Ctrl Pts',(-0.150991776994562,-0.0844534827151793,
0.412992742384559));
#18240=CARTESIAN_POINT('Ctrl Pts',(-0.0108540995180527,-0.172664692355881,
0.42093491050734));
#18241=CARTESIAN_POINT('Ctrl Pts',(0.139227048201004,-0.102697305280782,
0.428877078630119));
#18242=CARTESIAN_POINT('Ctrl Pts',(0.16176191642983,0.0613513639265466,
0.4368192467529));
#18243=CARTESIAN_POINT('Ctrl Pts',(0.0361062507758455,0.169195880912067,
0.444761414875679));
#18244=CARTESIAN_POINT('Ctrl Pts',(-0.12262644992489,0.12203958882886,0.45270358299846));
#18245=CARTESIAN_POINT('Ctrl Pts',(-0.169020724600573,-0.0369175042249048,
0.460645751121239));
#18246=CARTESIAN_POINT('Ctrl Pts',(-0.0605746513833496,-0.162054370729346,
0.468587919244019));
#18247=CARTESIAN_POINT('Ctrl Pts',(0.103364025571403,-0.138732785167649,
0.4765300873668));
#18248=CARTESIAN_POINT('Ctrl Pts',(0.172610636112938,0.0116822841681558,
0.484472255489579));
#18249=CARTESIAN_POINT('Ctrl Pts',(0.083728171010617,0.151395181039277,
0.49241442361236));
#18250=CARTESIAN_POINT('Ctrl Pts',(-0.081857900459256,0.152414538660527,
0.500356591735139));
#18251=CARTESIAN_POINT('Ctrl Pts',(-0.172453725526818,0.0138065207282529,
0.50829875985792));
#18252=CARTESIAN_POINT('Ctrl Pts',(-0.105064221167447,-0.137449688588867,
0.516240927980699));
#18253=CARTESIAN_POINT('Ctrl Pts',(0.0585749034388466,-0.162787862415564,
0.52418309610348));
#18254=CARTESIAN_POINT('Ctrl Pts',(0.168553398866689,-0.0389956304370821,
0.532125264226259));
#18255=CARTESIAN_POINT('Ctrl Pts',(0.124119664784058,0.120520605195094,
0.54006743234904));
#18256=CARTESIAN_POINT('Ctrl Pts',(-0.0340204335384149,0.16962758491636,
0.548009600471819));
#18257=CARTESIAN_POINT('Ctrl Pts',(-0.160994319687769,0.0633382703503284,
0.5559517685946));
#18258=CARTESIAN_POINT('Ctrl Pts',(-0.14048086942825,-0.100975406844349,
0.563893936717379));
#18259=CARTESIAN_POINT('Ctrl Pts',(0.00872748937560605,-0.172785237771916,
0.57183610484016));
#18260=CARTESIAN_POINT('Ctrl Pts',(0.149940571302356,-0.0863060399984934,
0.579778272962939));
#18261=CARTESIAN_POINT('Ctrl Pts',(0.153792685935992,0.0792383569699183,
0.58772044108572));
#18262=CARTESIAN_POINT('Ctrl Pts',(0.0167549005293281,0.17219227848818,
0.595662609208499));
#18263=CARTESIAN_POINT('Ctrl Pts',(-0.135632095058532,0.107400382926376,
0.60360477733128));
#18264=CARTESIAN_POINT('Ctrl Pts',(-0.163766157558233,-0.0557812970565469,
0.611546945454059));
#18265=CARTESIAN_POINT('Ctrl Pts',(-0.0418735953979919,-0.167861578305293,
0.61948911357684));
#18266=CARTESIAN_POINT('Ctrl Pts',(0.118379481984711,-0.126163408751231,
0.627431281699619));
#18267=CARTESIAN_POINT('Ctrl Pts',(0.17018479228316,0.0311134044783985,
0.6353734498224));
#18268=CARTESIAN_POINT('Ctrl Pts',(0.0660833491022344,0.159887142804326,
0.643315617945179));
#18269=CARTESIAN_POINT('Ctrl Pts',(-0.0985572308567358,0.142187832491218,
0.651257786067961));
#18270=CARTESIAN_POINT('Ctrl Pts',(-0.172909262181909,-0.00577013989488307,
0.659199954190738));
#18271=CARTESIAN_POINT('Ctrl Pts',(-0.0888586457050277,-0.148442071348278,
0.667142122313521));
#18272=CARTESIAN_POINT('Ctrl Pts',(0.0765956190331784,-0.155125815413241,
0.675084290436298));
#18273=CARTESIAN_POINT('Ctrl Pts',(0.171880427770071,-0.0196983758791502,
0.683026458559081));
#18274=CARTESIAN_POINT('Ctrl Pts',(0.109705106722326,0.133774799651286,
0.690968626681858));
#18275=CARTESIAN_POINT('Ctrl Pts',(-0.0529713625168984,0.164696515493808,
0.698910794804641));
#18276=CARTESIAN_POINT('Ctrl Pts',(-0.167120621735807,0.0447393032280997,
0.706852962927418));
#18277=CARTESIAN_POINT('Ctrl Pts',(-0.12817022249092,-0.116203707037801,
0.7147951310502));
#18278=CARTESIAN_POINT('Ctrl Pts',(0.0281972679828983,-0.17069218359667,
0.722737299172979));
#18279=CARTESIAN_POINT('Ctrl Pts',(0.158733164168978,-0.0688090841067,0.73067946729576));
#18280=CARTESIAN_POINT('Ctrl Pts',(0.14385317469873,0.0961102054508026,
0.738621635418538));
#18281=CARTESIAN_POINT('Ctrl Pts',(-0.00281110139369983,0.172982673038814,
0.746563803541321));
#18282=CARTESIAN_POINT('Ctrl Pts',(-0.146900119814081,0.0913852409380608,
0.754505971664098));
#18283=CARTESIAN_POINT('Ctrl Pts',(-0.156413536862055,-0.0739304602244656,
0.762448139786881));
#18284=CARTESIAN_POINT('Ctrl Pts',(-0.0226360851712103,-0.171518264656626,
0.770390307909658));
#18285=CARTESIAN_POINT('Ctrl Pts',(0.131878346029848,-0.111977717922496,
0.778332476032441));
#18286=CARTESIAN_POINT('Ctrl Pts',(0.165578663890314,0.0501459223366878,
0.786274644155218));
#18287=CARTESIAN_POINT('Ctrl Pts',(0.047591915084802,0.166330746049129,
0.794216812278001));
#18288=CARTESIAN_POINT('Ctrl Pts',(-0.113993917241593,0.130139518573781,
0.802158980400778));
#18289=CARTESIAN_POINT('Ctrl Pts',(-0.171149610334614,-0.0252728776558711,
0.81010114852356));
#18290=CARTESIAN_POINT('Ctrl Pts',(-0.0715146774936035,-0.157532721571376,
0.818043316646339));
#18291=CARTESIAN_POINT('Ctrl Pts',(0.0936350469135118,-0.14547640857611,
0.825985484769119));
#18292=CARTESIAN_POINT('Ctrl Pts',(0.173005448853992,-0.000148759965830227,
0.8339276528919));
#18293=CARTESIAN_POINT('Ctrl Pts',(0.0938850861191564,0.145315168055841,
0.841869821014678));
#18294=CARTESIAN_POINT('Ctrl Pts',(-0.0712436606821878,0.157655473343934,
0.849811989137461));
#18295=CARTESIAN_POINT('Ctrl Pts',(-0.171105895159299,0.0255671684868261,
0.857754157260238));
#18296=CARTESIAN_POINT('Ctrl Pts',(-0.114217551294,-0.129943289319231,0.86569632538302));
#18297=CARTESIAN_POINT('Ctrl Pts',(0.0473058035714782,-0.166412344527548,
0.873638493505798));
#18298=CARTESIAN_POINT('Ctrl Pts',(0.16549218245563,-0.0504305959589149,
0.88158066162858));
#18299=CARTESIAN_POINT('Ctrl Pts',(0.132070720552549,0.111750759440056,
0.889522829751358));
#18300=CARTESIAN_POINT('Ctrl Pts',(-0.022341089517305,0.171556938600217,
0.89746499787414));
#18301=CARTESIAN_POINT('Ctrl Pts',(-0.156286166401977,0.074199337288632,
0.905407165996919));
#18302=CARTESIAN_POINT('Ctrl Pts',(-0.147057058974526,-0.0911324797668838,
0.913349334119699));
#18303=CARTESIAN_POINT('Ctrl Pts',(-0.00310857778072832,-0.172977582960567,
0.92129150224248));
#18304=CARTESIAN_POINT('Ctrl Pts',(0.143687680016546,-0.0963574495000853,
0.929233670365259));
#18305=CARTESIAN_POINT('Ctrl Pts',(0.158851261322436,0.0685360068793772,
0.93717583848804));
#18306=CARTESIAN_POINT('Ctrl Pts',(0.0284907678468484,0.170643439985825,
0.945118006610819));
#18307=CARTESIAN_POINT('Ctrl Pts',(-0.127970195944242,0.116423951198588,
0.9530601747336));
#18308=CARTESIAN_POINT('Ctrl Pts',(-0.167197313372666,-0.0444518375735043,
0.961002342856378));
#18309=CARTESIAN_POINT('Ctrl Pts',(-0.0532545149190986,-0.164605176417482,
0.96894451097916));
#18310=CARTESIAN_POINT('Ctrl Pts',(0.10947489024455,-0.133963263130763,
0.976886679101939));
#18311=CARTESIAN_POINT('Ctrl Pts',(0.1719140491614,0.0194027617526574,0.984828847224719));
#18312=CARTESIAN_POINT('Ctrl Pts',(0.0768622776450996,0.154993863549195,
0.992771015347499));
#18313=CARTESIAN_POINT('Ctrl Pts',(-0.088603236555915,0.148594663210074,
1.00071318347028));
#18314=CARTESIAN_POINT('Ctrl Pts',(-0.172899083515371,0.00606748566075909,
1.00865535159306));
#18315=CARTESIAN_POINT('Ctrl Pts',(-0.0988016073770141,-0.142018132090297,
1.01659751971584));
#18316=CARTESIAN_POINT('Ctrl Pts',(0.0658082913934689,-0.160000550769587,
1.02453968783862));
#18317=CARTESIAN_POINT('Ctrl Pts',(0.170131034504888,-0.0314060274628177,
1.0324818559614));
#18318=CARTESIAN_POINT('Ctrl Pts',(0.118596271784576,0.125959643463681,
1.04042402408418));
#18319=CARTESIAN_POINT('Ctrl Pts',(-0.0415848597483297,0.167933340651612,
1.04836619220696));
#18320=CARTESIAN_POINT('Ctrl Pts',(-0.163669987576804,0.0560628453550813,
1.05630836032974));
#18321=CARTESIAN_POINT('Ctrl Pts',(-0.135816592328243,-0.107166975841641,
1.06425052845252));
#18322=CARTESIAN_POINT('Ctrl Pts',(0.0164587544616562,-0.172220837485682,
1.0721926965753));
#18323=CARTESIAN_POINT('Ctrl Pts',(0.153656191292587,-0.0795027190739688,
1.08013486469808));
#18324=CARTESIAN_POINT('Ctrl Pts',(0.150088771199207,0.0860480576341552,
1.08807703282086));
#18325=CARTESIAN_POINT('Ctrl Pts',(0.00902461748204118,0.172769973496559,
1.09601920094364));
#18326=CARTESIAN_POINT('Ctrl Pts',(-0.140307012982855,0.101216844302358,
1.10396136906642));
#18327=CARTESIAN_POINT('Ctrl Pts',(-0.161103005268346,-0.0630613126743013,
1.1119035371892));
#18328=CARTESIAN_POINT('Ctrl Pts',(-0.0343120939874615,-0.1695688287065,
1.11984570531198));
#18329=CARTESIAN_POINT('Ctrl Pts',(0.123912220401285,-0.120733877175888,
1.12778787343476));
#18330=CARTESIAN_POINT('Ctrl Pts',(0.168620210916381,0.0387057093103061,
1.13573004155754));
#18331=CARTESIAN_POINT('Ctrl Pts',(0.0588547652196237,0.162686889679659,
1.14367220968032));
#18332=CARTESIAN_POINT('Ctrl Pts',(-0.104827691798069,0.137630165643247,
1.1516143778031));
#18333=CARTESIAN_POINT('Ctrl Pts',(-0.172477213770776,-0.0135099294065116,
1.15955654592588));
#18334=CARTESIAN_POINT('Ctrl Pts',(-0.0821198886720452,-0.152273541192125,
1.16749871404866));
#18335=CARTESIAN_POINT('Ctrl Pts',(0.083467690946984,-0.15153894559049,
1.17544088217144));
#18336=CARTESIAN_POINT('Ctrl Pts',(0.172590290696882,-0.0119791076405788,
1.18338305029422));
#18337=CARTESIAN_POINT('Ctrl Pts',(0.103602453294194,0.13855482356859,1.191325218417));
#18338=CARTESIAN_POINT('Ctrl Pts',(-0.0602958748103966,0.162158302111078,
1.19926738653978));
#18339=CARTESIAN_POINT('Ctrl Pts',(-0.168956987158091,0.0372081167644847,
1.20720955466256));
#18340=CARTESIAN_POINT('Ctrl Pts',(-0.122836141658186,-0.121828526073448,
1.21515172278534));
#18341=CARTESIAN_POINT('Ctrl Pts',(0.0358152290369173,-0.169257723108079,
1.22309389090812));
#18342=CARTESIAN_POINT('Ctrl Pts',(0.161656170495932,-0.0616294572691503,
1.2310360590309));
#18343=CARTESIAN_POINT('Ctrl Pts',(0.13940345221127,0.102457722863032,1.23897822715368));
#18344=CARTESIAN_POINT('Ctrl Pts',(-0.0105571497596809,0.172683102970871,
1.24692039527646));
#18345=CARTESIAN_POINT('Ctrl Pts',(-0.150846317973597,0.0847130203482025,
1.25486256339924));
#18346=CARTESIAN_POINT('Ctrl Pts',(-0.152944761892581,-0.0808628918127005,
1.26280473152202));
#18347=CARTESIAN_POINT('Ctrl Pts',(-0.0149300913057054,-0.172360087712588,
1.2707468996448));
#18348=CARTESIAN_POINT('Ctrl Pts',(0.136762076743997,-0.105957736043287,
1.27868906776758));
#18349=CARTESIAN_POINT('Ctrl Pts',(0.163166132393764,0.0575127872937276,
1.28663123589036));
#18350=CARTESIAN_POINT('Ctrl Pts',(0.0400932480780463,0.168295688956082,
1.29457340401314));
#18351=CARTESIAN_POINT('Ctrl Pts',(-0.119709170414695,0.124902449862528,
1.30251557213592));
#18352=CARTESIAN_POINT('Ctrl Pts',(-0.169845690614082,-0.0329142650230248,
1.3104577402587));
#18353=CARTESIAN_POINT('Ctrl Pts',(-0.0643861093061943,-0.160578131733314,
1.31839990838148));
#18354=CARTESIAN_POINT('Ctrl Pts',(0.100057762773863,-0.141135932963798,
1.32634207650426));
#18355=CARTESIAN_POINT('Ctrl Pts',(0.172838444806952,0.00760127985757451,
1.33428424462704));
#18356=CARTESIAN_POINT('Ctrl Pts',(0.0872813550697656,0.149374939398002,
1.34222641274982));
#18357=CARTESIAN_POINT('Ctrl Pts',(-0.0782344227434143,0.154305808621531,
1.3501685808726));
#18358=CARTESIAN_POINT('Ctrl Pts',(-0.172079431848303,0.0178767046294837,
1.35811074899538));
#18359=CARTESIAN_POINT('Ctrl Pts',(-0.108282003268856,-0.134929297194493,
1.36605291711816));
#18360=CARTESIAN_POINT('Ctrl Pts',(0.0547128650701426,-0.164126201264144,
1.37399508524094));
#18361=CARTESIAN_POINT('Ctrl Pts',(0.167585127127835,-0.0429666431014547,
1.38193725336372));
#18362=CARTESIAN_POINT('Ctrl Pts',(0.126932197981417,0.117554773230619,
1.3898794214865));
#18363=CARTESIAN_POINT('Ctrl Pts',(-0.0300036684000219,0.170383942402052,
1.39782158960928));
#18364=CARTESIAN_POINT('Ctrl Pts',(-0.159453085214751,0.0671239123677834,
1.40576375773206));
#18365=CARTESIAN_POINT('Ctrl Pts',(-0.142827107870127,-0.0976285101620078,
1.41370592585484));
#18366=CARTESIAN_POINT('Ctrl Pts',(0.00464319840846943,-0.172943201171859,
1.42164809397762));
#18367=CARTESIAN_POINT('Ctrl Pts',(0.147859810582222,-0.0898241270588577,
1.4295902621004));
#18368=CARTESIAN_POINT('Ctrl Pts',(0.155621735944117,0.0755830265922534,
1.43753243022318));
#18369=CARTESIAN_POINT('Ctrl Pts',(0.0208179928734729,0.171748455656582,
1.44547459834596));
#18370=CARTESIAN_POINT('Ctrl Pts',(-0.133056846329205,0.11057447892796,
1.45341676646874));
#18371=CARTESIAN_POINT('Ctrl Pts',(-0.165038560097216,-0.0518967460486161,
1.46135893459152));
#18372=CARTESIAN_POINT('Ctrl Pts',(-0.0458268296361176,-0.166825854601292,
1.4693011027143));
#18373=CARTESIAN_POINT('Ctrl Pts',(0.115364766925686,-0.128924136976022,
1.47724327083708));
#18374=CARTESIAN_POINT('Ctrl Pts',(0.170874595884426,0.0270830477535184,
1.48518543895986));
#18375=CARTESIAN_POINT('Ctrl Pts',(0.0698377457337486,0.158283721017069,
1.49312760708264));
#18376=CARTESIAN_POINT('Ctrl Pts',(-0.0951624750893037,0.144471999488883,
1.50106977520542));
#18377=CARTESIAN_POINT('Ctrl Pts',(-0.173012914651864,-0.00167525885548286,
1.5090119433282));
#18378=CARTESIAN_POINT('Ctrl Pts',(-0.092311001583214,-0.14631755460685,
1.51695411145098));
#18379=CARTESIAN_POINT('Ctrl Pts',(0.072853104778531,-0.156861289272697,
1.52489627957376));
#18380=CARTESIAN_POINT('Ctrl Pts',(0.171475934783304,-0.0238129810547936,
1.53283844769654));
#18381=CARTESIAN_POINT('Ctrl Pts',(0.11261423476106,0.131269690464983,1.54078061581932));
#18382=CARTESIAN_POINT('Ctrl Pts',(0.00518264413773371,0.154149172621267,
1.54607539456784));
#18383=CARTESIAN_POINT('Ctrl Pts',(-0.0415060733757155,0.140340900570467,
1.5487227839421));
#18384=CARTESIAN_POINT('Ctrl Pts',(-0.146248097568756,-0.000123763188177425,
1.45893449541571));
#18385=CARTESIAN_POINT('Ctrl Pts',(-0.146367493381718,-0.0150081347743067,
1.45974264180765));
#18386=CARTESIAN_POINT('Ctrl Pts',(-0.144277648885518,-0.0298597803798721,
1.46055078819958));
#18387=CARTESIAN_POINT('Ctrl Pts',(-0.139839652725699,-0.043973059977961,
1.46135893459152));
#18388=CARTESIAN_POINT('Ctrl Pts',(-0.125301316610186,-0.0902064488995044,
1.46400632396578));
#18389=CARTESIAN_POINT('Ctrl Pts',(-0.08556407312315,-0.1285161517504,1.46665371334004));
#18390=CARTESIAN_POINT('Ctrl Pts',(-0.0388301852859989,-0.141354050238301,
1.4693011027143));
#18391=CARTESIAN_POINT('Ctrl Pts',(0.00790370255115092,-0.154191948726202,
1.47194849208856));
#18392=CARTESIAN_POINT('Ctrl Pts',(0.0616342347384179,-0.141558042851112,
1.47459588146282));
#18393=CARTESIAN_POINT('Ctrl Pts',(0.0977511389918415,-0.109239892458645,
1.47724327083708));
#18394=CARTESIAN_POINT('Ctrl Pts',(0.133868043245265,-0.0769217420661769,
1.47989066021134));
#18395=CARTESIAN_POINT('Ctrl Pts',(0.152371319564846,-0.024919347156331,
1.4825380495856));
#18396=CARTESIAN_POINT('Ctrl Pts',(0.144783482699524,0.0229486291758506,
1.48518543895986));
#18397=CARTESIAN_POINT('Ctrl Pts',(0.137195645834202,0.0708166055080336,
1.48783282833412));
#18398=CARTESIAN_POINT('Ctrl Pts',(0.103516695783975,0.114550163262552,
1.49048021770838));
#18399=CARTESIAN_POINT('Ctrl Pts',(0.0591771839550196,0.13411498855178,
1.49312760708264));
#18400=CARTESIAN_POINT('Ctrl Pts',(0.014837672126065,0.153679813841007,
1.4957749964569));
#18401=CARTESIAN_POINT('Ctrl Pts',(-0.0401624014816186,0.149075906664945,
1.49842238583116));
#18402=CARTESIAN_POINT('Ctrl Pts',(-0.0806375115458872,0.122416076686187,
1.50106977520542));
#18403=CARTESIAN_POINT('Ctrl Pts',(-0.0937869288003098,0.113754921033589,
1.50192985013695));
#18404=CARTESIAN_POINT('Ctrl Pts',(-0.105403311347291,0.102765876910903,
1.50278992506847));
#18405=CARTESIAN_POINT('Ctrl Pts',(-0.115078604842433,0.0902138214954038,
1.50365));
#18406=CARTESIAN_POINT('Ctrl Pts',(-0.0686146973663081,-0.0959584553529135,
1.07336015076065E-17));
#18407=CARTESIAN_POINT('Ctrl Pts',(-0.0712979561985307,-0.0944995001033786,
9.02613639135873E-18));
#18408=CARTESIAN_POINT('Ctrl Pts',(-0.0739152333025289,-0.0929325179580126,
1.64107321374712E-17));
#18409=CARTESIAN_POINT('Ctrl Pts',(-0.0764591723283171,-0.0912589988675934,
1.6154612370034E-17));
#18410=CARTESIAN_POINT('Ctrl Pts',(-0.0824897891353913,-0.0872917841461184,
1.52077426268717E-17));
#18411=CARTESIAN_POINT('Ctrl Pts',(-0.0881090519769445,-0.0827275518978924,
1.30971627060498E-17));
#18412=CARTESIAN_POINT('Ctrl Pts',(-0.0932912133381108,-0.0776621329443405,
1.43114686768087E-17));
#18413=CARTESIAN_POINT('Ctrl Pts',(-0.0960634919631888,-0.074952307504085,
1.49610807310118E-17));
#18414=CARTESIAN_POINT('Ctrl Pts',(-0.0987043519497191,-0.0721043812799658,
1.74993329480528E-17));
#18415=CARTESIAN_POINT('Ctrl Pts',(-0.101206237074718,-0.0691378820326018,
9.97465998686664E-18));
#18416=CARTESIAN_POINT('Ctrl Pts',(-0.105823426721714,-0.0636632543305198,
-3.91200561030858E-18));
#18417=CARTESIAN_POINT('Ctrl Pts',(-0.109972666997065,-0.0577811896139199,
2.24798207762934E-18));
#18418=CARTESIAN_POINT('Ctrl Pts',(-0.113625452403263,-0.0515741981665521,
9.54097911787244E-18));
#18419=CARTESIAN_POINT('Ctrl Pts',(-0.115386295340069,-0.0485820878086944,
1.30566037435822E-17));
#18420=CARTESIAN_POINT('Ctrl Pts',(-0.117027309103105,-0.0455212415157476,
-2.79521757168051E-18));
#18421=CARTESIAN_POINT('Ctrl Pts',(-0.118543833519887,-0.0424058589801268,
-3.46944695195361E-18));
#18422=CARTESIAN_POINT('Ctrl Pts',(-0.122700941917732,-0.0338659484069709,
-5.31764971597768E-18));
#18423=CARTESIAN_POINT('Ctrl Pts',(-0.125931492798984,-0.0249085743588085,
-1.15219401683824E-18));
#18424=CARTESIAN_POINT('Ctrl Pts',(-0.128167520083254,-0.0157105262534848,
9.54097911787244E-18));
#18425=CARTESIAN_POINT('Ctrl Pts',(-0.128992166906242,-0.0123182862745252,
1.3484621181291E-17));
#18426=CARTESIAN_POINT('Ctrl Pts',(-0.129681150280034,-0.00889298553317688,
1.10989611676181E-17));
#18427=CARTESIAN_POINT('Ctrl Pts',(-0.130229483957028,-0.00544263935519351,
9.54097911787244E-18));
#18428=CARTESIAN_POINT('Ctrl Pts',(-0.130761899349706,-0.00209245771889707,
8.02822573502553E-18));
#18429=CARTESIAN_POINT('Ctrl Pts',(-0.131160261982709,0.00127366115726457,
1.11791151702242E-17));
#18430=CARTESIAN_POINT('Ctrl Pts',(-0.131420990891747,0.00464012593483382,
8.67361737988404E-18));
#18431=CARTESIAN_POINT('Ctrl Pts',(-0.131728666658755,0.00861275649723166,
5.71697955546795E-18));
#18432=CARTESIAN_POINT('Ctrl Pts',(-0.131845259942619,0.0125891451047215,
-9.26473565962443E-18));
#18433=CARTESIAN_POINT('Ctrl Pts',(-0.131765781147177,0.0165567997877194,
-1.04083408558608E-17));
#18434=CARTESIAN_POINT('Ctrl Pts',(-0.131635692412819,0.0230509492424239,
-1.21888544026837E-17));
#18435=CARTESIAN_POINT('Ctrl Pts',(-0.13098103789945,0.0295216962360144,
-2.67049856555875E-17));
#18436=CARTESIAN_POINT('Ctrl Pts',(-0.129839098367345,0.0359278479980343,
-3.46944695195361E-17));
#18437=CARTESIAN_POINT('Ctrl Pts',(-0.129254890951344,0.0392051855997028,
-3.87818275556788E-17));
#18438=CARTESIAN_POINT('Ctrl Pts',(-0.128542951403208,0.0424656461998481,
-3.10678831811161E-17));
#18439=CARTESIAN_POINT('Ctrl Pts',(-0.1277070993652,0.0457037274559979,
-3.29597460435593E-17));
#18440=CARTESIAN_POINT('Ctrl Pts',(-0.126886363095037,0.0488832504000222,
-3.48173959609792E-17));
#18441=CARTESIAN_POINT('Ctrl Pts',(-0.125948031872817,0.0520333657183593,
-3.53366201082739E-17));
#18442=CARTESIAN_POINT('Ctrl Pts',(-0.124899042599898,0.0551436241923499,
-3.46944695195361E-17));
#18443=CARTESIAN_POINT('Ctrl Pts',(-0.122234979928128,0.0630425834229368,
-3.30636335736642E-17));
#18444=CARTESIAN_POINT('Ctrl Pts',(-0.118856305871375,0.070695441500891,
-2.1366080483524E-17));
#18445=CARTESIAN_POINT('Ctrl Pts',(-0.114834854776346,0.078019637496205,
-1.73472347597681E-17));
#18446=CARTESIAN_POINT('Ctrl Pts',(-0.11215901866562,0.0828930893082948,
-1.46731322388254E-17));
#18447=CARTESIAN_POINT('Ctrl Pts',(-0.109198005187061,0.0876211033078822,
8.28606628989234E-18));
#18448=CARTESIAN_POINT('Ctrl Pts',(-0.105966883726074,0.0921780034666525,
8.67361737988404E-18));
#18449=CARTESIAN_POINT('Ctrl Pts',(-0.104137243112614,0.094758373688769,
8.89307035390601E-18));
#18450=CARTESIAN_POINT('Ctrl Pts',(-0.102221042121924,0.0972831505018574,
-2.31209379389524E-17));
#18451=CARTESIAN_POINT('Ctrl Pts',(-0.100229777791505,0.0997373632832089,
-2.08166817117217E-17));
#18452=CARTESIAN_POINT('Ctrl Pts',(-0.0937202782075859,0.107760254486057,
-1.32840027382311E-17));
#18453=CARTESIAN_POINT('Ctrl Pts',(-0.0863914655699752,0.115060936709644,
5.4842312373535E-18));
#18454=CARTESIAN_POINT('Ctrl Pts',(-0.0783508402622743,0.121487309774744,
1.38777878078145E-17));
#18455=CARTESIAN_POINT('Ctrl Pts',(-0.073610711791116,0.125275800441382,
1.8825977152717E-17));
#18456=CARTESIAN_POINT('Ctrl Pts',(-0.068622257850438,0.128760167547443,
-9.09579695168528E-18));
#18457=CARTESIAN_POINT('Ctrl Pts',(-0.0634007094575209,0.131904027763685,
-6.93889390390723E-18));
#18458=CARTESIAN_POINT('Origin',(0.,0.,0.));
#18459=CARTESIAN_POINT('Origin',(-0.0721687836487033,-0.125,-0.3));
#18460=CARTESIAN_POINT('',(-0.0721687836487033,-0.125,-0.3));
#18461=CARTESIAN_POINT('',(0.0721687836487032,-0.125,-0.3));
#18462=CARTESIAN_POINT('',(-0.0360843918243517,-0.125,-0.3));
#18463=CARTESIAN_POINT('',(-0.0721687836487033,-0.125,-0.15));
#18464=CARTESIAN_POINT('',(-0.0721687836487033,-0.125,-0.3));
#18465=CARTESIAN_POINT('',(0.0721687836487032,-0.125,-0.15));
#18466=CARTESIAN_POINT('',(-0.0721687836487033,-0.125,-0.15));
#18467=CARTESIAN_POINT('',(0.0721687836487032,-0.125,-0.3));
#18468=CARTESIAN_POINT('Origin',(-0.144337567297406,1.76762539787485E-17,
-0.3));
#18469=CARTESIAN_POINT('',(-0.144337567297406,1.76762539787485E-17,-0.3));
#18470=CARTESIAN_POINT('',(-0.126295371385231,-0.03125,-0.3));
#18471=CARTESIAN_POINT('',(-0.144337567297406,2.77555756156289E-17,-0.15));
#18472=CARTESIAN_POINT('',(-0.144337567297406,1.76762539787485E-17,-0.3));
#18473=CARTESIAN_POINT('',(-0.144337567297406,1.76762539787485E-17,-0.15));
#18474=CARTESIAN_POINT('Origin',(-0.0721687836487032,0.125,-0.3));
#18475=CARTESIAN_POINT('',(-0.0721687836487032,0.125,-0.3));
#18476=CARTESIAN_POINT('',(-0.090210979560879,0.09375,-0.3));
#18477=CARTESIAN_POINT('',(-0.0721687836487032,0.125,-0.15));
#18478=CARTESIAN_POINT('',(-0.0721687836487032,0.125,-0.3));
#18479=CARTESIAN_POINT('',(-0.0721687836487032,0.125,-0.15));
#18480=CARTESIAN_POINT('Origin',(0.0721687836487032,0.125,-0.3));
#18481=CARTESIAN_POINT('',(0.0721687836487032,0.125,-0.3));
#18482=CARTESIAN_POINT('',(0.0360843918243516,0.125,-0.3));
#18483=CARTESIAN_POINT('',(0.0721687836487032,0.125,-0.15));
#18484=CARTESIAN_POINT('',(0.0721687836487032,0.125,-0.3));
#18485=CARTESIAN_POINT('',(0.0721687836487032,0.125,-0.15));
#18486=CARTESIAN_POINT('Origin',(0.144337567297406,0.,-0.3));
#18487=CARTESIAN_POINT('',(0.144337567297406,0.,-0.3));
#18488=CARTESIAN_POINT('',(0.126295371385231,0.03125,-0.3));
#18489=CARTESIAN_POINT('',(0.144337567297406,0.,-0.15));
#18490=CARTESIAN_POINT('',(0.144337567297406,0.,-0.3));
#18491=CARTESIAN_POINT('',(0.144337567297406,0.,-0.15));
#18492=CARTESIAN_POINT('Origin',(0.0721687836487032,-0.125,-0.3));
#18493=CARTESIAN_POINT('',(0.0902109795608791,-0.09375,-0.3));
#18494=CARTESIAN_POINT('',(0.0721687836487032,-0.125,-0.15));
#18495=CARTESIAN_POINT('Origin',(0.,0.,-0.15));
#18496=CARTESIAN_POINT('Origin',(0.,0.,0.));
#18497=CARTESIAN_POINT('',(-0.275,-3.36777869765522E-17,0.));
#18498=CARTESIAN_POINT('Origin',(0.,0.,0.));
#18499=CARTESIAN_POINT('Origin',(0.,0.,-0.3));
#18500=CARTESIAN_POINT('',(-0.275,-3.36777869765522E-17,-0.3));
#18501=CARTESIAN_POINT('',(-0.275,-3.36777869765522E-17,-0.3));
#18502=CARTESIAN_POINT('Origin',(0.,0.,-0.3));
#18503=CARTESIAN_POINT('Origin',(0.,0.,-0.3));
#18504=CARTESIAN_POINT('Origin',(0.,0.,1.6));
#18505=CARTESIAN_POINT('',(0.,0.,0.));
#18506=CARTESIAN_POINT('Origin',(0.,0.,0.12));
#18507=CARTESIAN_POINT('',(-0.12639138516214,8.91322620741042E-5,0.00934196736194174));
#18508=CARTESIAN_POINT('',(-0.12645,1.54856587752183E-17,-5.55111512312578E-17));
#18509=CARTESIAN_POINT('',(-0.12645,1.54856587752183E-17,0.12));
#18510=CARTESIAN_POINT('',(-0.0488748409397564,0.116622692573588,0.));
#18511=CARTESIAN_POINT('Origin',(0.,0.,0.));
#18512=CARTESIAN_POINT('Ctrl Pts',(-0.0489111879062984,0.116810626195002,
1.20007714660797E-17));
#18513=CARTESIAN_POINT('Ctrl Pts',(-0.0838963038512042,0.101957324585112,
0.00240024091002088));
#18514=CARTESIAN_POINT('Ctrl Pts',(-0.11198221847721,0.0702793053867637,
0.00480048182004174));
#18515=CARTESIAN_POINT('Ctrl Pts',(-0.122072221370749,0.0336561163696377,
0.00720072273006261));
#18516=CARTESIAN_POINT('Ctrl Pts',(-0.125072637487486,0.022765653033531,
0.00791447094068899));
#18517=CARTESIAN_POINT('Ctrl Pts',(-0.126481745582665,0.0114379076904012,
0.00862821915131536));
#18518=CARTESIAN_POINT('Ctrl Pts',(-0.12639138516214,8.91322620741042E-5,
0.00934196736194174));
#18519=CARTESIAN_POINT('Origin',(0.,0.,0.12));
#18520=CARTESIAN_POINT('',(-0.126396145829628,-9.95859796292312E-5,0.0593419673619417));
#18521=CARTESIAN_POINT('',(-0.126575671592806,-7.20628672610732E-5,0.0456580326380584));
#18522=CARTESIAN_POINT('',(-0.12645,1.54856587752183E-17,0.12));
#18523=CARTESIAN_POINT('',(-0.10808967569503,-0.0656218295092665,0.));
#18524=CARTESIAN_POINT('Ctrl Pts',(-0.126575671592806,-7.20628672610732E-5,
0.0456580326380584));
#18525=CARTESIAN_POINT('Ctrl Pts',(-0.126327459688109,0.0361497101693465,
0.0433719816070355));
#18526=CARTESIAN_POINT('Ctrl Pts',(-0.109912066394173,0.0725710138228805,
0.0410859305760125));
#18527=CARTESIAN_POINT('Ctrl Pts',(-0.0824515099939393,0.0961223418729112,
0.0387998795449896));
#18528=CARTESIAN_POINT('Ctrl Pts',(-0.05137998778939,0.122770586059505,
0.036213220908657));
#18529=CARTESIAN_POINT('Ctrl Pts',(-0.00616751748104999,0.132941603485868,
0.0336265622723243));
#18530=CARTESIAN_POINT('Ctrl Pts',(0.0333172074018229,0.122176268745047,
0.0310399036359917));
#18531=CARTESIAN_POINT('Ctrl Pts',(0.0728019322846963,0.111410934004226,
0.028453244999659));
#18532=CARTESIAN_POINT('Ctrl Pts',(0.106558911742102,0.0797092470962188,
0.0258665863633264));
#18533=CARTESIAN_POINT('Ctrl Pts',(0.11981357554495,0.0409763259700822,
0.0232799277269937));
#18534=CARTESIAN_POINT('Ctrl Pts',(0.133068239347797,0.00224340484394604,
0.0206932690906611));
#18535=CARTESIAN_POINT('Ctrl Pts',(0.125820587496086,-0.0435207505003201,
0.0181066104543285));
#18536=CARTESIAN_POINT('Ctrl Pts',(0.101166903546451,-0.0762076816581678,
0.0155199518179958));
#18537=CARTESIAN_POINT('Ctrl Pts',(0.0765132195968157,-0.108894612816016,
0.0129332931816632));
#18538=CARTESIAN_POINT('Ctrl Pts',(0.0344535035492562,-0.128504319787445,
0.0103466345453306));
#18539=CARTESIAN_POINT('Ctrl Pts',(-0.00636464094143544,-0.126469737202777,
0.00775997590899791));
#18540=CARTESIAN_POINT('Ctrl Pts',(-0.0471827854321269,-0.124435154618108,
0.00517331727266527));
#18541=CARTESIAN_POINT('Ctrl Pts',(-0.0867593583659505,-0.100756282477341,
0.00258665863633259));
#18542=CARTESIAN_POINT('Ctrl Pts',(-0.108089675695031,-0.0656218295092657,
-5.55111512312578E-17));
#18543=CARTESIAN_POINT('Origin',(0.,0.,0.));
#18544=CARTESIAN_POINT('Ctrl Pts',(-0.12639138516214,8.91322620741042E-5,
0.00934196736194174));
#18545=CARTESIAN_POINT('Ctrl Pts',(-0.126154274972366,-0.0296906128949183,
0.011214877787648));
#18546=CARTESIAN_POINT('Ctrl Pts',(-0.115592373032178,-0.0596151635265703,
0.0130877882133543));
#18547=CARTESIAN_POINT('Ctrl Pts',(-0.0963650578556872,-0.0821635787359664,
0.0149606986390606));
#18548=CARTESIAN_POINT('Ctrl Pts',(-0.0698103971670931,-0.113304978845907,
0.0175473572753932));
#18549=CARTESIAN_POINT('Ctrl Pts',(-0.0267272342632827,-0.130377059081323,
0.0201340159117258));
#18550=CARTESIAN_POINT('Ctrl Pts',(0.0139574509341311,-0.125868770046104,
0.0227206745480584));
#18551=CARTESIAN_POINT('Ctrl Pts',(0.0546421361315456,-0.121360481010885,
0.0253073331843911));
#18552=CARTESIAN_POINT('Ctrl Pts',(0.0929283436225635,-0.0952718227050311,
0.0278939918207237));
#18553=CARTESIAN_POINT('Ctrl Pts',(0.112018291148455,-0.0590635258734944,
0.0304806504570564));
#18554=CARTESIAN_POINT('Ctrl Pts',(0.131108238674346,-0.0228552290419586,
0.033067309093389));
#18555=CARTESIAN_POINT('Ctrl Pts',(0.131001926235112,0.0234727063152593,
0.0356539677297216));
#18556=CARTESIAN_POINT('Ctrl Pts',(0.111741771403992,0.0595891814911641,
0.0382406263660542));
#18557=CARTESIAN_POINT('Ctrl Pts',(0.0924816165728724,0.0957056566670696,
0.0408272850023869));
#18558=CARTESIAN_POINT('Ctrl Pts',(0.0540676193498672,0.121610671661662,
0.0434139436387195));
#18559=CARTESIAN_POINT('Ctrl Pts',(0.0133639835211523,0.125930636937597,
0.0460006022750522));
#18560=CARTESIAN_POINT('Ctrl Pts',(-0.0273396523075625,0.130250602213533,
0.0485872609113848));
#18561=CARTESIAN_POINT('Ctrl Pts',(-0.0703329267419868,0.112985517770812,
0.0511739195477175));
#18562=CARTESIAN_POINT('Ctrl Pts',(-0.0967449447385466,0.0817152626609385,
0.0537605781840501));
#18563=CARTESIAN_POINT('Ctrl Pts',(-0.115741878896724,0.0592240248649833,
0.0556210412433473));
#18564=CARTESIAN_POINT('Ctrl Pts',(-0.126160906676814,0.0294875554882879,
0.0574815043026445));
#18565=CARTESIAN_POINT('Ctrl Pts',(-0.126396145829628,-9.95859796292312E-5,
0.0593419673619417));
#18566=CARTESIAN_POINT('Origin',(0.,0.,0.12));
#18567=CARTESIAN_POINT('',(-0.126529791093031,9.025049583615E-5,0.109341967361942));
#18568=CARTESIAN_POINT('',(-0.126349242904067,8.85860673823967E-5,0.0956580326380584));
#18569=CARTESIAN_POINT('',(-0.12645,1.54856587752183E-17,0.12));
#18570=CARTESIAN_POINT('Ctrl Pts',(-0.126349242904067,8.85860673823967E-5,
0.0956580326380584));
#18571=CARTESIAN_POINT('Ctrl Pts',(-0.126441591528965,0.0135570965972842,
0.0948119253946973));
#18572=CARTESIAN_POINT('Ctrl Pts',(-0.124448136217638,0.0269990101701626,
0.0939658181513361));
#18573=CARTESIAN_POINT('Ctrl Pts',(-0.120249444863787,0.0397126388809939,
0.093119710907975));
#18574=CARTESIAN_POINT('Ctrl Pts',(-0.107413505522824,0.0785798365820317,
0.0905330522716423));
#18575=CARTESIAN_POINT('Ctrl Pts',(-0.0739673525896496,0.110640458354997,
0.0879463936353097));
#18576=CARTESIAN_POINT('Ctrl Pts',(-0.0345920580258737,0.121821308595361,
0.085359734998977));
#18577=CARTESIAN_POINT('Ctrl Pts',(0.00478323653790218,0.133002158835724,
0.0827730763626444));
#18578=CARTESIAN_POINT('Ctrl Pts',(0.0500876727322792,0.123303237543486,
0.0801864177263117));
#18579=CARTESIAN_POINT('Ctrl Pts',(0.0814342209129887,0.0969820390626645,
0.077599759089979));
#18580=CARTESIAN_POINT('Ctrl Pts',(0.112780769093698,0.0706608405818426,
0.0750131004536464));
#18581=CARTESIAN_POINT('Ctrl Pts',(0.13016942926074,0.0277173649124373,
0.0724264418173139));
#18582=CARTESIAN_POINT('Ctrl Pts',(0.12596827751407,-0.0129984006283456,
0.0698397831809812));
#18583=CARTESIAN_POINT('Ctrl Pts',(0.121767125767399,-0.0537141661691284,
0.0672531245446486));
#18584=CARTESIAN_POINT('Ctrl Pts',(0.0959761621070158,-0.0922022215812886,
0.0646664659083159));
#18585=CARTESIAN_POINT('Ctrl Pts',(0.059914723710966,-0.111567668284471,
0.0620798072719833));
#18586=CARTESIAN_POINT('Ctrl Pts',(0.0238532853149157,-0.130933114987654,
0.0594931486356506));
#18587=CARTESIAN_POINT('Ctrl Pts',(-0.0224786278168013,-0.131175952981858,
0.056906489999318));
#18588=CARTESIAN_POINT('Ctrl Pts',(-0.0587401909579078,-0.112190380850839,
0.0543198313629853));
#18589=CARTESIAN_POINT('Ctrl Pts',(-0.0950017540990138,-0.0932048087198191,
0.0517331727266527));
#18590=CARTESIAN_POINT('Ctrl Pts',(-0.12119296724951,-0.0549908264635757,
0.0491465140903201));
#18591=CARTESIAN_POINT('Ctrl Pts',(-0.125823286774378,-0.0143210998620416,
0.0465598554539874));
#18592=CARTESIAN_POINT('Ctrl Pts',(-0.126361397696569,-0.0095946821776348,
0.0462592478486778));
#18593=CARTESIAN_POINT('Ctrl Pts',(-0.12660831057823,-0.00483509759607578,
0.0459586402433681));
#18594=CARTESIAN_POINT('Ctrl Pts',(-0.126575671592806,-7.20628672610732E-5,
0.0456580326380584));
#18595=CARTESIAN_POINT('Ctrl Pts',(-0.126396145829628,-9.95859796292312E-5,
0.0593419673619417));
#18596=CARTESIAN_POINT('Ctrl Pts',(-0.12648796685852,-0.0116483513064931,
0.0600681629389771));
#18597=CARTESIAN_POINT('Ctrl Pts',(-0.125028206814926,-0.0231743653405588,
0.0607943585160125));
#18598=CARTESIAN_POINT('Ctrl Pts',(-0.121921363946098,-0.034237873926493,
0.0615205540930479));
#18599=CARTESIAN_POINT('Ctrl Pts',(-0.110855003598394,-0.0736453296270277,
0.0641072127293806));
#18600=CARTESIAN_POINT('Ctrl Pts',(-0.0788915213442898,-0.107184815251071,
0.0666938713657133));
#18601=CARTESIAN_POINT('Ctrl Pts',(-0.0400617348236378,-0.120133683626334,
0.069280530002046));
#18602=CARTESIAN_POINT('Ctrl Pts',(-0.00123194830298627,-0.133082552001597,
0.0718671886383786));
#18603=CARTESIAN_POINT('Ctrl Pts',(0.0444641424842127,-0.125440803128081,
0.0744538472747112));
#18604=CARTESIAN_POINT('Ctrl Pts',(0.0769682295152699,-0.100563001286921,
0.0770405059110438));
#18605=CARTESIAN_POINT('Ctrl Pts',(0.109472316546327,-0.0756851994457607,
0.0796271645473764));
#18606=CARTESIAN_POINT('Ctrl Pts',(0.128784399821243,-0.0335713446369571,
0.0822138231837091));
#18607=CARTESIAN_POINT('Ctrl Pts',(0.126427276285523,0.00729262199647547,
0.0848004818200417));
#18608=CARTESIAN_POINT('Ctrl Pts',(0.124070152749803,0.0481565886299079,
0.0873871404563744));
#18609=CARTESIAN_POINT('Ctrl Pts',(0.100043822403448,0.0877706670879697,
0.0899737990927071));
#18610=CARTESIAN_POINT('Ctrl Pts',(0.0648947831756147,0.108746049780439,
0.0925604577290397));
#18611=CARTESIAN_POINT('Ctrl Pts',(0.0297457439477817,0.129721432472907,
0.0951471163653723));
#18612=CARTESIAN_POINT('Ctrl Pts',(-0.0165260041615291,0.132058119399784,
0.0977337750017049));
#18613=CARTESIAN_POINT('Ctrl Pts',(-0.0536093211433369,0.114730442741844,
0.100320433638038));
#18614=CARTESIAN_POINT('Ctrl Pts',(-0.0906926381251451,0.0974027660839045,
0.10290709227437));
#18615=CARTESIAN_POINT('Ctrl Pts',(-0.11858752397945,0.0604107258411485,
0.105493750910703));
#18616=CARTESIAN_POINT('Ctrl Pts',(-0.12504939731921,0.0199921027543164,
0.108080409547035));
#18617=CARTESIAN_POINT('Ctrl Pts',(-0.126099919499473,0.0134211506765118,
0.108500928818671));
#18618=CARTESIAN_POINT('Ctrl Pts',(-0.126583971845017,0.00675963476331471,
0.108921448090306));
#18619=CARTESIAN_POINT('Ctrl Pts',(-0.126529791093031,9.025049583615E-5,
0.109341967361942));
#18620=CARTESIAN_POINT('Origin',(0.,0.,0.12));
#18621=CARTESIAN_POINT('',(-0.126296536029262,-6.10717992316628E-5,0.159341967361942));
#18622=CARTESIAN_POINT('',(-0.126453631260982,-0.000102348163238207,0.145658032638058));
#18623=CARTESIAN_POINT('',(-0.12645,1.54856587752183E-17,0.12));
#18624=CARTESIAN_POINT('Ctrl Pts',(-0.126453631260982,-0.000102348163238207,
0.145658032638058));
#18625=CARTESIAN_POINT('Ctrl Pts',(-0.126183364177612,0.031552920325249,
0.143665210546026));
#18626=CARTESIAN_POINT('Ctrl Pts',(-0.114073771100105,0.0633928690595716,
0.141672388453994));
#18627=CARTESIAN_POINT('Ctrl Pts',(-0.0925489356314354,0.0864391430514358,
0.139679566361962));
#18628=CARTESIAN_POINT('Ctrl Pts',(-0.0646099631645552,0.116352924063146,
0.13709290772563));
#18629=CARTESIAN_POINT('Ctrl Pts',(-0.0208084524006029,0.131451366650306,
0.134506249089297));
#18630=CARTESIAN_POINT('Ctrl Pts',(0.0196287675426836,0.125106932552633,
0.131919590452964));
#18631=CARTESIAN_POINT('Ctrl Pts',(0.0600659874859703,0.11876249845496,
0.129332931816632));
#18632=CARTESIAN_POINT('Ctrl Pts',(0.097138916608591,0.0909751876724545,
0.126746273180299));
#18633=CARTESIAN_POINT('Ctrl Pts',(0.114574233156503,0.0539423598350403,
0.124159614543967));
#18634=CARTESIAN_POINT('Ctrl Pts',(0.132009549704415,0.0169095319976262,
0.121572955907634));
#18635=CARTESIAN_POINT('Ctrl Pts',(0.129807253677619,-0.0293688128946969,
0.118986297271301));
#18636=CARTESIAN_POINT('Ctrl Pts',(0.108934072954415,-0.0645786240759305,
0.116399638634969));
#18637=CARTESIAN_POINT('Ctrl Pts',(0.0880608922312115,-0.099788435257164,
0.113812979998636));
#18638=CARTESIAN_POINT('Ctrl Pts',(0.0485168268116012,-0.123929712727308,
0.111226321362303));
#18639=CARTESIAN_POINT('Ctrl Pts',(0.00765986125275547,-0.126405537442516,
0.108639662725971));
#18640=CARTESIAN_POINT('Ctrl Pts',(-0.0331971043060904,-0.128881362157723,
0.106053004089638));
#18641=CARTESIAN_POINT('Ctrl Pts',(-0.0753669700041717,-0.109691734117994,
0.103466345453305));
#18642=CARTESIAN_POINT('Ctrl Pts',(-0.100339039978837,-0.0772600332835736,
0.100879686816973));
#18643=CARTESIAN_POINT('Ctrl Pts',(-0.117142637704978,-0.0554368822612891,
0.0991391354240014));
#18644=CARTESIAN_POINT('Ctrl Pts',(-0.126159269908366,-0.0276178718881664,
0.0973985840310299));
#18645=CARTESIAN_POINT('Ctrl Pts',(-0.126349242904067,8.85860673823967E-5,
0.0956580326380584));
#18646=CARTESIAN_POINT('Ctrl Pts',(-0.126529791093031,9.025049583615E-5,
0.109341967361942));
#18647=CARTESIAN_POINT('Ctrl Pts',(-0.126250700293628,-0.0342644551610371,
0.111508106726639));
#18648=CARTESIAN_POINT('Ctrl Pts',(-0.111690189779818,-0.0688279388928191,
0.113674246091336));
#18649=CARTESIAN_POINT('Ctrl Pts',(-0.0867076257192948,-0.092297473337895,
0.115840385456033));
#18650=CARTESIAN_POINT('Ctrl Pts',(-0.0568751199544048,-0.120323220412367,
0.118427044092366));
#18651=CARTESIAN_POINT('Ctrl Pts',(-0.0121812475994092,-0.132529508630403,
0.121013702728699));
#18652=CARTESIAN_POINT('Ctrl Pts',(0.0277554439013372,-0.123558363290506,
0.123600361365031));
#18653=CARTESIAN_POINT('Ctrl Pts',(0.0676921354020838,-0.114587217950609,
0.126187020001364));
#18654=CARTESIAN_POINT('Ctrl Pts',(0.102871646048582,-0.0844386390527785,
0.128773678637697));
#18655=CARTESIAN_POINT('Ctrl Pts',(0.117851793294146,-0.0463464242807743,
0.131360337274029));
#18656=CARTESIAN_POINT('Ctrl Pts',(0.13283194053971,-0.00825420950877041,
0.133946995910362));
#18657=CARTESIAN_POINT('Ctrl Pts',(0.127612724384341,0.0377816411374068,
0.136533654546694));
#18658=CARTESIAN_POINT('Ctrl Pts',(0.104485135941302,0.0715534408109559,
0.139120313183027));
#18659=CARTESIAN_POINT('Ctrl Pts',(0.0813575474982633,0.105325240484505,
0.14170697181936));
#18660=CARTESIAN_POINT('Ctrl Pts',(0.0403215867675544,0.126832989185426,
0.144293630455692));
#18661=CARTESIAN_POINT('Ctrl Pts',(-0.000609841963000384,0.126635909896556,
0.146880289092025));
#18662=CARTESIAN_POINT('Ctrl Pts',(-0.0415412706935549,0.126438830607686,
0.149466947728358));
#18663=CARTESIAN_POINT('Ctrl Pts',(-0.0823681674239554,0.104536923329025,
0.15205360636469));
#18664=CARTESIAN_POINT('Ctrl Pts',(-0.10516942503222,0.0705438627883669,
0.154640265001023));
#18665=CARTESIAN_POINT('Ctrl Pts',(-0.118984510025511,0.0499477610899654,
0.156207499121329));
#18666=CARTESIAN_POINT('Ctrl Pts',(-0.126182304652747,0.0249129445447297,
0.157774733241635));
#18667=CARTESIAN_POINT('Ctrl Pts',(-0.126296536029262,-6.10717992316628E-5,
0.159341967361942));
#18668=CARTESIAN_POINT('Origin',(0.,0.,0.12));
#18669=CARTESIAN_POINT('',(-0.126625441102054,2.7778768752873E-5,0.209341967361942));
#18670=CARTESIAN_POINT('',(-0.126471935391749,0.000101176582396995,0.195658032638058));
#18671=CARTESIAN_POINT('',(-0.12645,1.54856587752183E-17,0.12));
#18672=CARTESIAN_POINT('',(0.0958116152722397,0.0825211298936481,0.24));
#18673=CARTESIAN_POINT('Ctrl Pts',(-0.126625441102054,2.7778768752873E-5,
0.209341967361942));
#18674=CARTESIAN_POINT('Ctrl Pts',(-0.126482885932031,-0.0388928622545336,
0.21180133566563));
#18675=CARTESIAN_POINT('Ctrl Pts',(-0.107125339127294,-0.077921419747323,
0.214260703969318));
#18676=CARTESIAN_POINT('Ctrl Pts',(-0.0759952538809665,-0.101287130411732,
0.216720072273006));
#18677=CARTESIAN_POINT('Ctrl Pts',(-0.0432539585932993,-0.12586218783339,
0.219306730909339));
#18678=CARTESIAN_POINT('Ctrl Pts',(0.0025100419330305,-0.133111106253138,
0.221893389545672));
#18679=CARTESIAN_POINT('Ctrl Pts',(0.0412155518054008,-0.119764891216682,
0.224480048182004));
#18680=CARTESIAN_POINT('Ctrl Pts',(0.0799210616777711,-0.106418676180227,
0.227066706818337));
#18681=CARTESIAN_POINT('Ctrl Pts',(0.111568080896182,-0.072477327687567,
0.229653365454669));
#18682=CARTESIAN_POINT('Ctrl Pts',(0.122246574267713,-0.0330282462555153,
0.232240024091002));
#18683=CARTESIAN_POINT('Ctrl Pts',(0.132925067639245,0.00642083517653631,
0.234826682727335));
#18684=CARTESIAN_POINT('Ctrl Pts',(0.122635035163896,0.0513776495479799,
0.237413341363667));
#18685=CARTESIAN_POINT('Ctrl Pts',(0.0958116152722397,0.0825211298936481,
0.24));
#18686=CARTESIAN_POINT('',(-0.0959791030802601,0.0826138105732953,0.24));
#18687=CARTESIAN_POINT('Origin',(0.,0.,0.24));
#18688=CARTESIAN_POINT('Ctrl Pts',(-0.0959791030802601,0.0826138105732953,
0.24));
#18689=CARTESIAN_POINT('Ctrl Pts',(-0.0710417758635208,0.111296717646776,
0.237599759089979));
#18690=CARTESIAN_POINT('Ctrl Pts',(-0.0322351762885183,0.128218895525122,
0.235199518179958));
#18691=CARTESIAN_POINT('Ctrl Pts',(0.00571352152256588,0.126497857083363,
0.232799277269937));
#18692=CARTESIAN_POINT('Ctrl Pts',(0.0466095526337785,0.124643152028446,
0.230212618633605));
#18693=CARTESIAN_POINT('Ctrl Pts',(0.0865092470399708,0.101136876245298,
0.227625959997272));
#18694=CARTESIAN_POINT('Ctrl Pts',(0.107920636628548,0.0662586835305903,
0.225039301360939));
#18695=CARTESIAN_POINT('Ctrl Pts',(0.129332026217125,0.0313804908158828,
0.222452642724607));
#18696=CARTESIAN_POINT('Ctrl Pts',(0.132255110988087,-0.014869618830384,
0.219865984088274));
#18697=CARTESIAN_POINT('Ctrl Pts',(0.115395215428634,-0.0521699181865619,
0.217279325451942));
#18698=CARTESIAN_POINT('Ctrl Pts',(0.0985353198691812,-0.0894702175427398,
0.214692666815609));
#18699=CARTESIAN_POINT('Ctrl Pts',(0.0618924439793129,-0.117820706608829,
0.212106008179276));
#18700=CARTESIAN_POINT('Ctrl Pts',(0.0215571925812854,-0.12478734248304,
0.209519349542944));
#18701=CARTESIAN_POINT('Ctrl Pts',(-0.0187780588167422,-0.13175397835725,
0.206932690906611));
#18702=CARTESIAN_POINT('Ctrl Pts',(-0.0628056857229291,-0.117336761039583,
0.204346032270278));
#18703=CARTESIAN_POINT('Ctrl Pts',(-0.0912027768750998,-0.0878586653637446,
0.201759373633946));
#18704=CARTESIAN_POINT('Ctrl Pts',(-0.113530209130371,-0.0646812849521466,
0.199725593301983));
#18705=CARTESIAN_POINT('Ctrl Pts',(-0.126194825294183,-0.0321932513395888,
0.197691812970021));
#18706=CARTESIAN_POINT('Ctrl Pts',(-0.126471935391749,0.000101176582396995,
0.195658032638058));
#18707=CARTESIAN_POINT('Origin',(0.,0.,0.350421172358873));
#18708=CARTESIAN_POINT('',(-0.154453350152392,-8.79343647196378E-5,0.0295788276411275));
#18709=CARTESIAN_POINT('',(-0.15422847552802,0.000108763211052777,0.025421172358873));
#18710=CARTESIAN_POINT('',(-0.1543,-1.01731279388251E-15,0.350421172358873));
#18711=CARTESIAN_POINT('',(0.15408394018464,-0.00816268198427004,0.));
#18712=CARTESIAN_POINT('Ctrl Pts',(-0.15422847552802,0.000108763211052763,
0.025421172358873));
#18713=CARTESIAN_POINT('Ctrl Pts',(-0.154338737393477,0.0139570514561378,
0.0247074241482466));
#18714=CARTESIAN_POINT('Ctrl Pts',(-0.146387882101843,0.0778735560251454,
0.0214070173012875));
#18715=CARTESIAN_POINT('Ctrl Pts',(-0.0581466660421577,0.171532975008042,
0.0155199518179959));
#18716=CARTESIAN_POINT('Ctrl Pts',(0.109502662757235,0.144085240745689,
0.00775997590899784));
#18717=CARTESIAN_POINT('Ctrl Pts',(0.156737212705124,0.0419221657566679,
0.00258665863633264));
#18718=CARTESIAN_POINT('Ctrl Pts',(0.15408394018464,-0.00816268198427004,
0.));
#18719=CARTESIAN_POINT('',(0.129620323775263,-0.0841289546921688,3.62607491890453E-17));
#18720=CARTESIAN_POINT('Origin',(0.,0.,0.));
#18721=CARTESIAN_POINT('Ctrl Pts',(-0.154453350152392,-8.7934364719636E-5,
0.0295788276411275));
#18722=CARTESIAN_POINT('Ctrl Pts',(-0.154150470777978,0.0441115087317509,
0.0272927766101045));
#18723=CARTESIAN_POINT('Ctrl Pts',(-0.111454882743928,0.138841433785012,
0.0224200669427489));
#18724=CARTESIAN_POINT('Ctrl Pts',(0.0476444145610997,0.174632482457551,
0.0149606986390605));
#18725=CARTESIAN_POINT('Ctrl Pts',(0.168251138196633,0.0613688951001999,
0.0073871404563744));
#18726=CARTESIAN_POINT('Ctrl Pts',(0.154676764047789,-0.0451013867871701,
0.00240024091002087));
#18727=CARTESIAN_POINT('Ctrl Pts',(0.129620323775263,-0.0841289546921688,
1.57209315010398E-17));
#18728=CARTESIAN_POINT('Origin',(0.,0.,0.350421172358873));
#18729=CARTESIAN_POINT('',(-0.154177051641736,0.000108096719625833,0.0795788276411275));
#18730=CARTESIAN_POINT('',(-0.154234284709463,-0.000121519309271207,0.075421172358873));
#18731=CARTESIAN_POINT('',(-0.1543,-1.01731279388251E-15,0.350421172358873));
#18732=CARTESIAN_POINT('Ctrl Pts',(-0.154234284709463,-0.000121519309271208,
0.0754211723588731));
#18733=CARTESIAN_POINT('Ctrl Pts',(-0.153947235272697,0.0359820467524117,
0.0735607092995758));
#18734=CARTESIAN_POINT('Ctrl Pts',(-0.123557126730793,0.122717061869437,
0.0691135876039459));
#18735=CARTESIAN_POINT('Ctrl Pts',(0.0191012565771036,0.180005302104073,
0.0620798072719832));
#18736=CARTESIAN_POINT('Ctrl Pts',(0.159724738700703,0.0851738948996701,
0.0543198313629854));
#18737=CARTESIAN_POINT('Ctrl Pts',(0.160113920417758,-0.0844204212478698,
0.0465598554539874));
#18738=CARTESIAN_POINT('Ctrl Pts',(0.0199582426985643,-0.179924098035372,
0.0387998795449896));
#18739=CARTESIAN_POINT('Ctrl Pts',(-0.123251388539896,-0.123176028715441,
0.0317536518466181));
#18740=CARTESIAN_POINT('Ctrl Pts',(-0.153939142967466,-0.0362298265692857,
0.0272940827845792));
#18741=CARTESIAN_POINT('Ctrl Pts',(-0.15422847552802,0.000108763211052763,
0.025421172358873));
#18742=CARTESIAN_POINT('Ctrl Pts',(-0.154177051641736,0.000108096719625859,
0.0795788276411275));
#18743=CARTESIAN_POINT('Ctrl Pts',(-0.154289739603949,0.0165429814548096,
0.0787327203977663));
#18744=CARTESIAN_POINT('Ctrl Pts',(-0.144420757340354,0.0830897487115299,
0.0752999545180725));
#18745=CARTESIAN_POINT('Ctrl Pts',(-0.0494457976037486,0.174130301808973,
0.0692805300020459));
#18746=CARTESIAN_POINT('Ctrl Pts',(0.11640175885633,0.13862511662766,0.061520554093048));
#18747=CARTESIAN_POINT('Ctrl Pts',(0.18005704388064,-0.0185795878987759,
0.0537605781840501));
#18748=CARTESIAN_POINT('Ctrl Pts',(0.0856431484406112,-0.159474177462153,
0.0460006022750521));
#18749=CARTESIAN_POINT('Ctrl Pts',(-0.0839657292871194,-0.160363143120653,
0.0382406263660544));
#18750=CARTESIAN_POINT('Ctrl Pts',(-0.151599316432495,-0.0616831513139142,
0.0327667014880793));
#18751=CARTESIAN_POINT('Ctrl Pts',(-0.154493177716258,-0.00590000442131094,
0.0298794352464371));
#18752=CARTESIAN_POINT('Ctrl Pts',(-0.154453350152392,-8.7934364719636E-5,
0.0295788276411275));
#18753=CARTESIAN_POINT('Origin',(0.,0.,0.350421172358873));
#18754=CARTESIAN_POINT('',(-0.154304431028624,-0.000124889850439479,0.129578827641127));
#18755=CARTESIAN_POINT('',(-0.154397364694779,0.000110127730384366,0.125421172358873));
#18756=CARTESIAN_POINT('',(-0.1543,-1.01731279388251E-15,0.350421172358873));
#18757=CARTESIAN_POINT('Ctrl Pts',(-0.154397364694779,0.000110127730384357,
0.125421172358873));
#18758=CARTESIAN_POINT('Ctrl Pts',(-0.154463478494948,0.00824841157753406,
0.125000653087238));
#18759=CARTESIAN_POINT('Ctrl Pts',(-0.150239588102603,0.0663774823757793,
0.121993475179269));
#18760=CARTESIAN_POINT('Ctrl Pts',(-0.0766286530280003,0.163994611436961,
0.116399638634969));
#18761=CARTESIAN_POINT('Ctrl Pts',(0.0927599764682439,0.155440618724813,
0.108639662725971));
#18762=CARTESIAN_POINT('Ctrl Pts',(0.180714016146597,0.0104239566588842,
0.100879686816973));
#18763=CARTESIAN_POINT('Ctrl Pts',(0.11001758793024,-0.143743725357685,
0.093119710907975));
#18764=CARTESIAN_POINT('Ctrl Pts',(-0.0572637123892103,-0.171718146500831,
0.0853597349989769));
#18765=CARTESIAN_POINT('Ctrl Pts',(-0.146220320052713,-0.0783754111826042,
0.0794602221492764));
#18766=CARTESIAN_POINT('Ctrl Pts',(-0.154346328875204,-0.0142138442593302,
0.0761473679359084));
#18767=CARTESIAN_POINT('Ctrl Pts',(-0.154234284709463,-0.000121519309271208,
0.0754211723588731));
#18768=CARTESIAN_POINT('Ctrl Pts',(-0.154304431028624,-0.000124889850439474,
0.129578827641127));
#18769=CARTESIAN_POINT('Ctrl Pts',(-0.153974638929265,0.0385022981904757,
0.127586005549095));
#18770=CARTESIAN_POINT('Ctrl Pts',(-0.120018027207353,0.127784966030512,
0.123006524820731));
#18771=CARTESIAN_POINT('Ctrl Pts',(0.0280571680938306,0.178826694862324,
0.115840385456033));
#18772=CARTESIAN_POINT('Ctrl Pts',(0.163771354656592,0.0771047007047774,
0.108080409547035));
#18773=CARTESIAN_POINT('Ctrl Pts',(0.155709331479018,-0.0923080778690166,
0.100320433638038));
#18774=CARTESIAN_POINT('Ctrl Pts',(0.0109489686262093,-0.180682908560435,
0.0925604577290397));
#18775=CARTESIAN_POINT('Ctrl Pts',(-0.126591758993125,-0.118094248159534,
0.0856465890634029));
#18776=CARTESIAN_POINT('Ctrl Pts',(-0.153945238013925,-0.0337005743957639,
0.0813193790340989));
#18777=CARTESIAN_POINT('Ctrl Pts',(-0.154177051641736,0.000108096719625859,
0.0795788276411275));
#18778=CARTESIAN_POINT('Origin',(0.,0.,0.350421172358873));
#18779=CARTESIAN_POINT('',(-0.154326766555531,0.000123460234585843,0.179578827641127));
#18780=CARTESIAN_POINT('',(-0.154112736333057,-7.45225671948511E-5,0.175421172358873));
#18781=CARTESIAN_POINT('',(-0.1543,-1.01731279388251E-15,0.350421172358873));
#18782=CARTESIAN_POINT('Ctrl Pts',(-0.154112736333057,-7.45225671948471E-5,
0.175421172358873));
#18783=CARTESIAN_POINT('Ctrl Pts',(-0.153973346049181,0.0303998999070902,
0.173853938238567));
#18784=CARTESIAN_POINT('Ctrl Pts',(-0.130694151755309,0.111367805862998,
0.169700045481928));
#18785=CARTESIAN_POINT('Ctrl Pts',(-0.000871711368246156,0.181012066871201,
0.162959494088956));
#18786=CARTESIAN_POINT('Ctrl Pts',(0.149350085565286,0.102277888352765,
0.155199518179958));
#18787=CARTESIAN_POINT('Ctrl Pts',(0.168456255263351,-0.0662471829332422,
0.14743954227096));
#18788=CARTESIAN_POINT('Ctrl Pts',(0.0396733728729688,-0.17661315503135,
0.139679566361963));
#18789=CARTESIAN_POINT('Ctrl Pts',(-0.115072782317819,-0.134350623919955,
0.1323401097246));
#18790=CARTESIAN_POINT('Ctrl Pts',(-0.154056805498669,-0.041811035439686,
0.12758731172357));
#18791=CARTESIAN_POINT('Ctrl Pts',(-0.154397364694779,0.000110127730384357,
0.125421172358873));
#18792=CARTESIAN_POINT('Ctrl Pts',(-0.154326766555531,0.000123460234585825,
0.179578827641127));
#18793=CARTESIAN_POINT('Ctrl Pts',(-0.154418689716183,0.0108361910665024,
0.179025949336757));
#18794=CARTESIAN_POINT('Ctrl Pts',(-0.148597337680631,0.071569631208062,
0.175886412396054));
#18795=CARTESIAN_POINT('Ctrl Pts',(-0.0683530255288039,0.167611467503216,
0.170160216819019));
#18796=CARTESIAN_POINT('Ctrl Pts',(0.100397202365132,0.150621028353064,
0.162400240910021));
#18797=CARTESIAN_POINT('Ctrl Pts',(0.18100910679194,0.00139719974911195,
0.154640265001023));
#18798=CARTESIAN_POINT('Ctrl Pts',(0.102711092909207,-0.149052183789333,
0.146880289092025));
#18799=CARTESIAN_POINT('Ctrl Pts',(-0.0657574679958034,-0.168648048308422,
0.139120313183027));
#18800=CARTESIAN_POINT('Ctrl Pts',(-0.148058381688037,-0.0731761882111772,
0.133353159366061));
#18801=CARTESIAN_POINT('Ctrl Pts',(-0.154402705029802,-0.0116353181791797,
0.130172664185428));
#18802=CARTESIAN_POINT('Ctrl Pts',(-0.154304431028624,-0.000124889850439474,
0.129578827641127));
#18803=CARTESIAN_POINT('Origin',(0.,0.,0.350421172358873));
#18804=CARTESIAN_POINT('',(-0.154128406284035,-0.000157308197905263,0.229578827641128));
#18805=CARTESIAN_POINT('',(-0.154514081154978,3.38969080117728E-5,0.225421172358873));
#18806=CARTESIAN_POINT('',(-0.1543,-1.01731279388251E-15,0.350421172358873));
#18807=CARTESIAN_POINT('',(-0.0398513841857245,-0.149064942821851,0.24));
#18808=CARTESIAN_POINT('Ctrl Pts',(-0.0398513841857245,-0.149064942821851,
0.24));
#18809=CARTESIAN_POINT('Ctrl Pts',(-0.0883048112969314,-0.136111285829332,
0.237413341363667));
#18810=CARTESIAN_POINT('Ctrl Pts',(-0.143745772087175,-0.0847488633265083,
0.233939617244043));
#18811=CARTESIAN_POINT('Ctrl Pts',(-0.154234229255939,-0.017399338864059,
0.230465893124419));
#18812=CARTESIAN_POINT('Ctrl Pts',(-0.154128406284035,-0.00015730819790527,
0.229578827641128));
#18813=CARTESIAN_POINT('',(0.0399565498027962,-0.149273502906638,0.24));
#18814=CARTESIAN_POINT('Origin',(0.,0.,0.24));
#18815=CARTESIAN_POINT('Ctrl Pts',(0.0399565498027963,-0.149273502906638,
0.24));
#18816=CARTESIAN_POINT('Ctrl Pts',(-0.00490373130458673,-0.161043406468747,
0.237599759089979));
#18817=CARTESIAN_POINT('Ctrl Pts',(-0.107666111297752,-0.141562671532916,
0.23274014987627));
#18818=CARTESIAN_POINT('Ctrl Pts',(-0.154340128899266,-0.0474588267763927,
0.227880540662561));
#18819=CARTESIAN_POINT('Ctrl Pts',(-0.154514081154978,3.3896908011755E-5,
0.225421172358873));
#18820=CARTESIAN_POINT('Origin',(0.,0.,0.350421172358873));
#18821=CARTESIAN_POINT('Ctrl Pts',(-0.154514081154978,3.3896908011755E-5,
0.225421172358873));
#18822=CARTESIAN_POINT('Ctrl Pts',(-0.154523084458981,0.00249199339844659,
0.225293882026228));
#18823=CARTESIAN_POINT('Ctrl Pts',(-0.153375868586475,0.0548933889046004,
0.222579933057251));
#18824=CARTESIAN_POINT('Ctrl Pts',(-0.0942515706791253,0.154556313135293,
0.217279325451942));
#18825=CARTESIAN_POINT('Ctrl Pts',(0.0750450248431312,0.164716481511431,
0.209519349542944));
#18826=CARTESIAN_POINT('Ctrl Pts',(0.178461260043253,0.0303012077178856,
0.201759373633945));
#18827=CARTESIAN_POINT('Ctrl Pts',(0.125203781387627,-0.130731709675357,
0.193999397724948));
#18828=CARTESIAN_POINT('Ctrl Pts',(-0.0379704533096903,-0.17698585337688,
0.18623942181595));
#18829=CARTESIAN_POINT('Ctrl Pts',(-0.141587477595567,-0.0899051669249145,
0.180046680027258));
#18830=CARTESIAN_POINT('Ctrl Pts',(-0.154203404262525,-0.019896942829432,
0.176440596874899));
#18831=CARTESIAN_POINT('Ctrl Pts',(-0.154112736333057,-7.45225671948471E-5,
0.175421172358873));
#18832=CARTESIAN_POINT('Ctrl Pts',(-0.154128406284035,-0.00015730819790527,
0.229578827641128));
#18833=CARTESIAN_POINT('Ctrl Pts',(-0.153925652370292,0.0328779499839183,
0.227879234488086));
#18834=CARTESIAN_POINT('Ctrl Pts',(-0.127638532780061,0.116591914860373,
0.223592982698713));
#18835=CARTESIAN_POINT('Ctrl Pts',(0.00818767200092134,0.180778621679153,
0.216720072273006));
#18836=CARTESIAN_POINT('Ctrl Pts',(0.154249898498561,0.0947283641859207,
0.208960096364008));
#18837=CARTESIAN_POINT('Ctrl Pts',(0.164950538597243,-0.0745810526211722,
0.201200120455011));
#18838=CARTESIAN_POINT('Ctrl Pts',(0.0308106631569891,-0.178364693496558,
0.193440144546012));
#18839=CARTESIAN_POINT('Ctrl Pts',(-0.118879635670858,-0.129347344159377,
0.186233046941385));
#18840=CARTESIAN_POINT('Ctrl Pts',(-0.153988624301243,-0.0392836590090855,
0.18161260797309));
#18841=CARTESIAN_POINT('Ctrl Pts',(-0.154326766555531,0.000123460234585825,
0.179578827641127));
#18842=CARTESIAN_POINT('Ctrl Pts',(0.0958116152722397,0.0825211298936481,
0.24));
#18843=CARTESIAN_POINT('Ctrl Pts',(0.122635035163896,0.0513776495479799,
0.237413341363667));
#18844=CARTESIAN_POINT('Ctrl Pts',(0.143215100114593,-0.0385359791949074,
0.232240024091002));
#18845=CARTESIAN_POINT('Ctrl Pts',(0.0482740424593604,-0.140360024672886,
0.224480048182004));
#18846=CARTESIAN_POINT('Ctrl Pts',(-0.0890179591196291,-0.118613269413641,
0.216720072273006));
#18847=CARTESIAN_POINT('Ctrl Pts',(-0.148173729266643,0.00709031985706173,
0.208960096364008));
#18848=CARTESIAN_POINT('Ctrl Pts',(-0.0772398646297824,0.126660050524678,
0.20120012045501));
#18849=CARTESIAN_POINT('Ctrl Pts',(0.0614999571705377,0.134986384232796,
0.193440144546013));
#18850=CARTESIAN_POINT('Ctrl Pts',(0.146250332679645,0.0248320655601208,
0.185680168637014));
#18851=CARTESIAN_POINT('Ctrl Pts',(0.102605431992647,-0.107135610424167,
0.177920192728017));
#18852=CARTESIAN_POINT('Ctrl Pts',(-0.0311170694815965,-0.145041225920327,
0.170160216819019));
#18853=CARTESIAN_POINT('Ctrl Pts',(-0.137521919612742,-0.0556176253575994,
0.162400240910021));
#18854=CARTESIAN_POINT('Ctrl Pts',(-0.123195064154356,0.0826350160503635,
0.154640265001023));
#18855=CARTESIAN_POINT('Ctrl Pts',(-0.000714373963154436,0.148340737886347,
0.146880289092025));
#18856=CARTESIAN_POINT('Ctrl Pts',(0.122393508228972,0.0838174917835845,
0.139120313183027));
#18857=CARTESIAN_POINT('Ctrl Pts',(0.138051156695079,-0.0542900601549481,
0.131360337274029));
#18858=CARTESIAN_POINT('Ctrl Pts',(0.032512624755586,-0.14473579684844,
0.123600361365031));
#18859=CARTESIAN_POINT('Ctrl Pts',(-0.101568992309399,-0.108116932194331,
0.115840385456033));
#18860=CARTESIAN_POINT('Ctrl Pts',(-0.146482409833755,0.0234186855983926,
0.108080409547036));
#18861=CARTESIAN_POINT('Ctrl Pts',(-0.0627977522708403,0.13439480632666,
0.100320433638038));
#18862=CARTESIAN_POINT('Ctrl Pts',(0.076017492057093,0.127384745546031,
0.0925604577290397));
#18863=CARTESIAN_POINT('Ctrl Pts',(0.148096483096158,0.00854251017184644,
0.0848004818200417));
#18864=CARTESIAN_POINT('Ctrl Pts',(0.0901602332714121,-0.117799054254564,
0.0770405059110438));
#18865=CARTESIAN_POINT('Ctrl Pts',(-0.0469280390901857,-0.140724300875114,
0.069280530002046));
#18866=CARTESIAN_POINT('Ctrl Pts',(-0.142818485852497,-0.0401058440029853,
0.0615205540930479));
#18867=CARTESIAN_POINT('Ctrl Pts',(-0.113326201176411,0.0957204333280909,
0.0537605781840501));
#18868=CARTESIAN_POINT('Ctrl Pts',(0.0156536221268617,0.147515686656254,
0.0460006022750521));
#18869=CARTESIAN_POINT('Ctrl Pts',(0.130895613795878,0.0698006416724775,
0.0382406263660543));
#18870=CARTESIAN_POINT('Ctrl Pts',(0.13121455111358,-0.0691831643991777,
0.0304806504570563));
#18871=CARTESIAN_POINT('Ctrl Pts',(0.0163559286405278,-0.147449139316739,
0.0227206745480584));
#18872=CARTESIAN_POINT('Ctrl Pts',(-0.112893560070904,-0.0962328986104914,
0.0149606986390606));
#18873=CARTESIAN_POINT('Ctrl Pts',(-0.142972035491037,0.0393992613429074,
0.00720072273006258));
#18874=CARTESIAN_POINT('Ctrl Pts',(-0.0476516261894416,0.140572551456688,
-0.000559253178935252));
#18875=CARTESIAN_POINT('Ctrl Pts',(0.0897382482543901,0.118078928660352,
-0.00831922908793326));
#18876=CARTESIAN_POINT('Ctrl Pts',(0.128447313976429,0.0343555272840613,
-0.0134925463605985));
#18877=CARTESIAN_POINT('Ctrl Pts',(0.126272937371016,-0.00668937872268922,
-0.0160792049969311));
#18878=CARTESIAN_POINT('Ctrl Pts',(0.102845629995666,0.0885794229410663,
0.245359734998977));
#18879=CARTESIAN_POINT('Ctrl Pts',(0.13163829265517,0.0551495423644061,
0.242773076362644));
#18880=CARTESIAN_POINT('Ctrl Pts',(0.153729244145676,-0.0413651001137901,
0.237599759089979));
#18881=CARTESIAN_POINT('Ctrl Pts',(0.0518180837997932,-0.150664563191773,
0.229839783180981));
#18882=CARTESIAN_POINT('Ctrl Pts',(-0.0955532172229155,-0.127321268762976,
0.222079807271983));
#18883=CARTESIAN_POINT('Ctrl Pts',(-0.159051911315084,0.00761085605850937,
0.214319831362985));
#18884=CARTESIAN_POINT('Ctrl Pts',(-0.0829104333128967,0.135958804728216,
0.206559855453988));
#18885=CARTESIAN_POINT('Ctrl Pts',(0.0660149797280689,0.144896416659008,
0.19879987954499));
#18886=CARTESIAN_POINT('Ctrl Pts',(0.156987308467515,0.0266551129460425,
0.191039903635992));
#18887=CARTESIAN_POINT('Ctrl Pts',(0.110138215124307,-0.11500097684123,
0.183279927726994));
#18888=CARTESIAN_POINT('Ctrl Pts',(-0.0334015307576278,-0.155689435072511,
0.175519951817996));
#18889=CARTESIAN_POINT('Ctrl Pts',(-0.147618098500879,-0.0597007962188336,
0.167759975908998));
#18890=CARTESIAN_POINT('Ctrl Pts',(-0.13223943620312,0.0887016700559064,
0.16));
#18891=CARTESIAN_POINT('Ctrl Pts',(-0.000766819764851659,0.159231180881298,
0.152240024091002));
#18892=CARTESIAN_POINT('Ctrl Pts',(0.131379034007743,0.0899709573066447,
0.144480048182004));
#18893=CARTESIAN_POINT('Ctrl Pts',(0.14818618955117,-0.0582757677477129,
0.136720072273006));
#18894=CARTESIAN_POINT('Ctrl Pts',(0.0348995407947136,-0.15536158290941,
0.128960096364009));
#18895=CARTESIAN_POINT('Ctrl Pts',(-0.109025685167754,-0.116054342400242,
0.12120012045501));
#18896=CARTESIAN_POINT('Ctrl Pts',(-0.157236423577976,0.0251379696208395,
0.113440144546013));
#18897=CARTESIAN_POINT('Ctrl Pts',(-0.0674080525232269,0.144261408030094,
0.105680168637014));
#18898=CARTESIAN_POINT('Ctrl Pts',(0.0815983201941432,0.136736703272292,
0.0979201927280168));
#18899=CARTESIAN_POINT('Ctrl Pts',(0.158968994112971,0.00916965900085902,
0.0901602168190187));
#18900=CARTESIAN_POINT('Ctrl Pts',(0.0967793514910216,-0.126447277955604,
0.0824002409100209));
#18901=CARTESIAN_POINT('Ctrl Pts',(-0.0503732635231939,-0.151055582750353,
0.0746402650010229));
#18902=CARTESIAN_POINT('Ctrl Pts',(-0.15330351242688,-0.0430502166284845,
0.066880289092025));
#18903=CARTESIAN_POINT('Ctrl Pts',(-0.121646050135849,0.102747753924341,
0.0591203131830272));
#18904=CARTESIAN_POINT('Ctrl Pts',(0.0168028336102756,0.158345558472194,
0.0513603372740292));
#18905=CARTESIAN_POINT('Ctrl Pts',(0.140505322097486,0.074925059414875,
0.0436003613650313));
#18906=CARTESIAN_POINT('Ctrl Pts',(0.140847674214973,-0.0742622500154084,
0.0358403854560334));
#18907=CARTESIAN_POINT('Ctrl Pts',(0.0175566999932067,-0.158274125556283,
0.0280804095470355));
#18908=CARTESIAN_POINT('Ctrl Pts',(-0.121181646661057,-0.103297841872129,
0.0203204336380376));
#18909=CARTESIAN_POINT('Ctrl Pts',(-0.153468334920127,0.0422917601656304,
0.0125604577290396));
#18910=CARTESIAN_POINT('Ctrl Pts',(-0.0511499728070136,0.150892692640473,
0.00480048182004178));
#18911=CARTESIAN_POINT('Ctrl Pts',(0.0963263864220051,0.126747699355464,
-0.00295949408895622));
#18912=CARTESIAN_POINT('Ctrl Pts',(0.137877280219327,0.0368777401082635,
-0.00813281136162143));
#18913=CARTESIAN_POINT('Ctrl Pts',(0.135543271642224,-0.00718047980988283,
-0.0107194699979541));
#18914=CARTESIAN_POINT('Ctrl Pts',(0.109879644719093,0.0946377159884845,
0.250719469997954));
#18915=CARTESIAN_POINT('Ctrl Pts',(0.140641550146443,0.0589214351808321,
0.248132811361621));
#18916=CARTESIAN_POINT('Ctrl Pts',(0.164243388176759,-0.0441942210326729,
0.242959494088956));
#18917=CARTESIAN_POINT('Ctrl Pts',(0.055362125140226,-0.160969101710661,
0.235199518179958));
#18918=CARTESIAN_POINT('Ctrl Pts',(-0.102088475326202,-0.13602926811231,
0.227439542270961));
#18919=CARTESIAN_POINT('Ctrl Pts',(-0.169930093363525,0.00813139225995705,
0.219679566361962));
#18920=CARTESIAN_POINT('Ctrl Pts',(-0.0885810019960112,0.145257558931755,
0.211919590452965));
#18921=CARTESIAN_POINT('Ctrl Pts',(0.0705300022856002,0.154806449085219,
0.204159614543967));
#18922=CARTESIAN_POINT('Ctrl Pts',(0.167724284255384,0.0284781603319641,
0.196399638634969));
#18923=CARTESIAN_POINT('Ctrl Pts',(0.117670998255967,-0.122866343258294,
0.188639662725971));
#18924=CARTESIAN_POINT('Ctrl Pts',(-0.0356859920336591,-0.166337644224695,
0.180879686816973));
#18925=CARTESIAN_POINT('Ctrl Pts',(-0.157714277389017,-0.0637839670800676,
0.173119710907975));
#18926=CARTESIAN_POINT('Ctrl Pts',(-0.141283808251885,0.0947683240614489,
0.165359734998977));
#18927=CARTESIAN_POINT('Ctrl Pts',(-0.000819265566548849,0.17012162387625,
0.157599759089979));
#18928=CARTESIAN_POINT('Ctrl Pts',(0.140364559786514,0.0961244228297045,
0.149839783180981));
#18929=CARTESIAN_POINT('Ctrl Pts',(0.158321222407261,-0.0622614753404775,
0.142079807271983));
#18930=CARTESIAN_POINT('Ctrl Pts',(0.0372864568338413,-0.16598736897038,
0.134319831362986));
#18931=CARTESIAN_POINT('Ctrl Pts',(-0.116482378026109,-0.123991752606152,
0.126559855453987));
#18932=CARTESIAN_POINT('Ctrl Pts',(-0.167990437322196,0.0268572536432864,
0.11879987954499));
#18933=CARTESIAN_POINT('Ctrl Pts',(-0.0720183527756138,0.154128009733527,
0.111039903635992));
#18934=CARTESIAN_POINT('Ctrl Pts',(0.0871791483311938,0.146088660998552,
0.103279927726994));
#18935=CARTESIAN_POINT('Ctrl Pts',(0.169841505129784,0.00979680782987164,
0.0955199518179957));
#18936=CARTESIAN_POINT('Ctrl Pts',(0.103398469710631,-0.135095501656644,
0.0877599759089979));
#18937=CARTESIAN_POINT('Ctrl Pts',(-0.0538184879562023,-0.161386864625592,
0.08));
#18938=CARTESIAN_POINT('Ctrl Pts',(-0.163788539001263,-0.0459945892539838,
0.0722400240910021));
#18939=CARTESIAN_POINT('Ctrl Pts',(-0.129965899095288,0.10977507452059,
0.0644800481820042));
#18940=CARTESIAN_POINT('Ctrl Pts',(0.0179520450936897,0.169175430288133,
0.0567200722730062));
#18941=CARTESIAN_POINT('Ctrl Pts',(0.150115030399095,0.0800494771572726,
0.0489600963640084));
#18942=CARTESIAN_POINT('Ctrl Pts',(0.150480797316365,-0.0793413356316391,
0.0412001204550104));
#18943=CARTESIAN_POINT('Ctrl Pts',(0.0187574713458855,-0.169099111795828,
0.0334401445460125));
#18944=CARTESIAN_POINT('Ctrl Pts',(-0.129469733251211,-0.110362785133767,
0.0256801686370146));
#18945=CARTESIAN_POINT('Ctrl Pts',(-0.163964634349217,0.0451842589883535,
0.0179201927280167));
#18946=CARTESIAN_POINT('Ctrl Pts',(-0.0546483194245858,0.161212833824257,
0.0101602168190188));
#18947=CARTESIAN_POINT('Ctrl Pts',(0.10291452458962,0.135416470050577,0.00240024091002082));
#18948=CARTESIAN_POINT('Ctrl Pts',(0.147307246462226,0.0393999529324658,
-0.00277307636264439));
#18949=CARTESIAN_POINT('Ctrl Pts',(0.144813605913432,-0.00767158089707644,
-0.00535973499897704));
#18950=CARTESIAN_POINT('Ctrl Pts',(0.116913659442519,0.100696009035903,
0.256079204996931));
#18951=CARTESIAN_POINT('Ctrl Pts',(0.149644807637716,0.0626933279972582,
0.253492546360598));
#18952=CARTESIAN_POINT('Ctrl Pts',(0.174757532207842,-0.0470233419515556,
0.248319229087933));
#18953=CARTESIAN_POINT('Ctrl Pts',(0.0589061664806588,-0.171273640229548,
0.240559253178935));
#18954=CARTESIAN_POINT('Ctrl Pts',(-0.108623733429488,-0.144737267461644,
0.232799277269938));
#18955=CARTESIAN_POINT('Ctrl Pts',(-0.180808275411966,0.00865192846140473,
0.225039301360939));
#18956=CARTESIAN_POINT('Ctrl Pts',(-0.0942515706791253,0.154556313135293,
0.217279325451942));
#18957=CARTESIAN_POINT('Ctrl Pts',(0.0750450248431312,0.164716481511431,
0.209519349542944));
#18958=CARTESIAN_POINT('Ctrl Pts',(0.178461260043253,0.0303012077178856,
0.201759373633945));
#18959=CARTESIAN_POINT('Ctrl Pts',(0.125203781387627,-0.130731709675357,
0.193999397724948));
#18960=CARTESIAN_POINT('Ctrl Pts',(-0.0379704533096903,-0.17698585337688,
0.18623942181595));
#18961=CARTESIAN_POINT('Ctrl Pts',(-0.167810456277154,-0.0678671379413016,
0.178479445906952));
#18962=CARTESIAN_POINT('Ctrl Pts',(-0.150328180300649,0.100834978066992,
0.170719469997954));
#18963=CARTESIAN_POINT('Ctrl Pts',(-0.000871711368246156,0.181012066871201,
0.162959494088956));
#18964=CARTESIAN_POINT('Ctrl Pts',(0.149350085565286,0.102277888352765,
0.155199518179958));
#18965=CARTESIAN_POINT('Ctrl Pts',(0.168456255263351,-0.0662471829332422,
0.14743954227096));
#18966=CARTESIAN_POINT('Ctrl Pts',(0.0396733728729688,-0.17661315503135,
0.139679566361963));
#18967=CARTESIAN_POINT('Ctrl Pts',(-0.123939070884463,-0.131929162812062,
0.131919590452964));
#18968=CARTESIAN_POINT('Ctrl Pts',(-0.178744451066417,0.0285765376657333,
0.124159614543967));
#18969=CARTESIAN_POINT('Ctrl Pts',(-0.0766286530280003,0.163994611436961,
0.116399638634969));
#18970=CARTESIAN_POINT('Ctrl Pts',(0.0927599764682439,0.155440618724813,
0.108639662725971));
#18971=CARTESIAN_POINT('Ctrl Pts',(0.180714016146597,0.0104239566588842,
0.100879686816973));
#18972=CARTESIAN_POINT('Ctrl Pts',(0.11001758793024,-0.143743725357685,
0.093119710907975));
#18973=CARTESIAN_POINT('Ctrl Pts',(-0.0572637123892103,-0.171718146500831,
0.0853597349989769));
#18974=CARTESIAN_POINT('Ctrl Pts',(-0.174273565575645,-0.048938961879483,
0.0775997590899791));
#18975=CARTESIAN_POINT('Ctrl Pts',(-0.138285748054726,0.11680239511684,
0.0698397831809812));
#18976=CARTESIAN_POINT('Ctrl Pts',(0.0191012565771036,0.180005302104073,
0.0620798072719832));
#18977=CARTESIAN_POINT('Ctrl Pts',(0.159724738700703,0.0851738948996701,
0.0543198313629854));
#18978=CARTESIAN_POINT('Ctrl Pts',(0.160113920417758,-0.0844204212478698,
0.0465598554539874));
#18979=CARTESIAN_POINT('Ctrl Pts',(0.0199582426985643,-0.179924098035372,
0.0387998795449896));
#18980=CARTESIAN_POINT('Ctrl Pts',(-0.137757819841364,-0.117427728395404,
0.0310399036359917));
#18981=CARTESIAN_POINT('Ctrl Pts',(-0.174460933778308,0.0480767578110765,
0.0232799277269937));
#18982=CARTESIAN_POINT('Ctrl Pts',(-0.0581466660421577,0.171532975008042,
0.0155199518179959));
#18983=CARTESIAN_POINT('Ctrl Pts',(0.109502662757235,0.144085240745689,
0.00775997590899784));
#18984=CARTESIAN_POINT('Ctrl Pts',(0.156737212705124,0.0419221657566679,
0.00258665863633264));
#18985=CARTESIAN_POINT('Ctrl Pts',(0.15408394018464,-0.00816268198427004,
0.));
#18986=CARTESIAN_POINT('Ctrl Pts',(0.15408394018464,-0.00816268198427004,
0.));
#18987=CARTESIAN_POINT('Ctrl Pts',(0.153697863146473,0.00250812953454787,
1.45220469349306E-17));
#18988=CARTESIAN_POINT('Ctrl Pts',(0.152123106309386,0.0130673133993916,
-2.32988231788825E-17));
#18989=CARTESIAN_POINT('Ctrl Pts',(0.149466152202855,0.0233620190894148,
-6.07153216591882E-17));
#18990=CARTESIAN_POINT('Ctrl Pts',(0.14793019248835,0.0293132898222067,
-8.23454409684948E-17));
#18991=CARTESIAN_POINT('Ctrl Pts',(0.146031563681721,0.0351760135160456,
3.17823908273165E-17));
#18992=CARTESIAN_POINT('Ctrl Pts',(0.143784059453749,0.0409171473780902,
6.24500451351651E-17));
#18993=CARTESIAN_POINT('Ctrl Pts',(0.142595904075608,0.0439522291322952,
7.86626679846993E-17));
#18994=CARTESIAN_POINT('Ctrl Pts',(0.141309213132582,0.0469553015723855,
1.03399090950918E-16));
#18995=CARTESIAN_POINT('Ctrl Pts',(0.13992871365498,0.0499144025840292,
1.00613961606655E-16));
#18996=CARTESIAN_POINT('Ctrl Pts',(0.135493978469587,0.0594202586791481,
9.16669744478229E-17));
#18997=CARTESIAN_POINT('Ctrl Pts',(0.130119641392827,0.0684241765595774,
5.76730757846686E-17));
#18998=CARTESIAN_POINT('Ctrl Pts',(0.123887660540245,0.0767683201192124,
1.38777878078145E-16));
#18999=CARTESIAN_POINT('Ctrl Pts',(0.120656388342022,0.0810947453345699,
1.808305895663E-16));
#19000=CARTESIAN_POINT('Ctrl Pts',(0.117193874983239,0.0852432898306738,
1.062697842984E-16));
#19001=CARTESIAN_POINT('Ctrl Pts',(0.11350808038867,0.0891875047540603,
1.14491749414469E-16));
#19002=CARTESIAN_POINT('Ctrl Pts',(0.110158526423333,0.0927719043720516,
1.21963656801269E-16));
#19003=CARTESIAN_POINT('Ctrl Pts',(0.106618991420749,0.0961915975683434,
1.17223950247179E-16));
#19004=CARTESIAN_POINT('Ctrl Pts',(0.102922970874274,0.0994011657423757,
1.02348685082632E-16));
#19005=CARTESIAN_POINT('Ctrl Pts',(0.0973787571548163,0.104215676830788,
8.00350512245867E-17));
#19006=CARTESIAN_POINT('Ctrl Pts',(0.0914754811895955,0.108568278221023,
6.56075743842472E-17));
#19007=CARTESIAN_POINT('Ctrl Pts',(0.0852365492443714,0.11239450959967,
3.29597460435593E-17));
#19008=CARTESIAN_POINT('Ctrl Pts',(0.0787787796913796,0.116354950379705,
-7.26807264206779E-19));
#19009=CARTESIAN_POINT('Ctrl Pts',(0.0719608771003193,0.11975150351845,
7.81983513604452E-17));
#19010=CARTESIAN_POINT('Ctrl Pts',(0.0648645680501024,0.122569786811788,
1.05818132034585E-16));
#19011=CARTESIAN_POINT('Ctrl Pts',(0.0619760396963809,0.123716959397427,
1.17060669392563E-16));
#19012=CARTESIAN_POINT('Ctrl Pts',(0.0590419697559043,0.124767587801255,
-1.70921410850511E-17));
#19013=CARTESIAN_POINT('Ctrl Pts',(0.0560804949635964,0.12571697313192,
-8.67361737988404E-19));
#19014=CARTESIAN_POINT('Ctrl Pts',(0.0481895916857994,0.128246627558523,
4.23638569993146E-17));
#19015=CARTESIAN_POINT('Ctrl Pts',(0.040081547172159,0.13006877931966,2.48189907303608E-17));
#19016=CARTESIAN_POINT('Ctrl Pts',(0.0318655688619291,0.131172622122806,
0.));
#19017=CARTESIAN_POINT('Ctrl Pts',(0.0267717292715239,0.131856995664207,
-1.5387571972871E-17));
#19018=CARTESIAN_POINT('Ctrl Pts',(0.0216363184326117,0.132264755542675,
5.61228976213782E-17));
#19019=CARTESIAN_POINT('Ctrl Pts',(0.0164863123329273,0.132388468809724,
3.03576608295941E-17));
#19020=CARTESIAN_POINT('Ctrl Pts',(0.0120733572364389,0.13249447666326,
8.27985532573229E-18));
#19021=CARTESIAN_POINT('Ctrl Pts',(0.00764667637530932,0.132391154756805,
7.9933444120104E-17));
#19022=CARTESIAN_POINT('Ctrl Pts',(0.00324855819595315,0.132074892239241,
9.62771529167128E-17));
#19023=CARTESIAN_POINT('Ctrl Pts',(-0.00215998367955725,0.131685971569047,
1.16375665467493E-16));
#19024=CARTESIAN_POINT('Ctrl Pts',(-0.00753310453775717,0.130975837616781,
1.12286849362194E-16));
#19025=CARTESIAN_POINT('Ctrl Pts',(-0.0128378223015392,0.129936202211006,
1.27068494615301E-16));
#19026=CARTESIAN_POINT('Ctrl Pts',(-0.0180922709275414,0.128906418710228,
1.41710064449709E-16));
#19027=CARTESIAN_POINT('Ctrl Pts',(-0.023283936630727,0.12755123862641,
1.19281234835921E-16));
#19028=CARTESIAN_POINT('Ctrl Pts',(-0.028350637156304,0.125868914531291,
9.19403442267708E-17));
#19029=CARTESIAN_POINT('Ctrl Pts',(-0.0326437071621008,0.124443463179602,
6.87741127091605E-17));
#19030=CARTESIAN_POINT('Ctrl Pts',(-0.0368509055758185,0.122782751372096,
3.08039683582783E-17));
#19031=CARTESIAN_POINT('Ctrl Pts',(-0.0409513668396969,0.120880349084932,
-1.95156391047391E-18));
#19032=CARTESIAN_POINT('Ctrl Pts',(-0.0436523616789034,0.119627226953286,
-2.45035827619675E-17));
#19033=CARTESIAN_POINT('Ctrl Pts',(-0.0463070048384274,0.118269169850402,
-4.56986185075063E-18));
#19034=CARTESIAN_POINT('Ctrl Pts',(-0.0489111879062984,0.116810626195002,
-1.73472347597681E-18));
#19035=CARTESIAN_POINT('Ctrl Pts',(0.0958116152722397,0.0825211298936481,
0.24));
#19036=CARTESIAN_POINT('Ctrl Pts',(0.102494250906434,0.0762804363331629,
0.24));
#19037=CARTESIAN_POINT('Ctrl Pts',(0.108399952301676,0.0693089192431419,
0.24));
#19038=CARTESIAN_POINT('Ctrl Pts',(0.113520383394708,0.0617855200816623,
0.24));
#19039=CARTESIAN_POINT('Ctrl Pts',(0.11760088593285,0.0557900777417299,
0.24));
#19040=CARTESIAN_POINT('Ctrl Pts',(0.1211824537664,0.0494427873910869,0.24));
#19041=CARTESIAN_POINT('Ctrl Pts',(0.124247292533427,0.0428169095598754,
0.24));
#19042=CARTESIAN_POINT('Ctrl Pts',(0.125635784531567,0.0398151273949318,
0.24));
#19043=CARTESIAN_POINT('Ctrl Pts',(0.126914357096627,0.0367636074968772,
0.24));
#19044=CARTESIAN_POINT('Ctrl Pts',(0.128080244072735,0.0336751552254939,
0.24));
#19045=CARTESIAN_POINT('Ctrl Pts',(0.13155694143068,0.024465331227027,0.24));
#19046=CARTESIAN_POINT('Ctrl Pts',(0.134041462136676,0.0149150332268467,
0.24));
#19047=CARTESIAN_POINT('Ctrl Pts',(0.135496608205084,0.00520422800883078,
0.24));
#19048=CARTESIAN_POINT('Ctrl Pts',(0.136052940597398,0.00149158663520877,
0.24));
#19049=CARTESIAN_POINT('Ctrl Pts',(0.136458356591543,-0.00224482315054724,
0.24));
#19050=CARTESIAN_POINT('Ctrl Pts',(0.136708928272429,-0.00599574054845843,
0.24));
#19051=CARTESIAN_POINT('Ctrl Pts',(0.136894600108428,-0.00877514370161729,
0.24));
#19052=CARTESIAN_POINT('Ctrl Pts',(0.136994942037659,-0.0115613689854128,
0.24));
#19053=CARTESIAN_POINT('Ctrl Pts',(0.137008733057845,-0.0143405417274864,
0.24));
#19054=CARTESIAN_POINT('Ctrl Pts',(0.137045731231951,-0.0217964308202384,
0.24));
#19055=CARTESIAN_POINT('Ctrl Pts',(0.136462408227525,-0.0292204075226799,
0.24));
#19056=CARTESIAN_POINT('Ctrl Pts',(0.135240454646173,-0.0365388974416549,
0.24));
#19057=CARTESIAN_POINT('Ctrl Pts',(0.134058793448489,-0.0436160693529878,
0.24));
#19058=CARTESIAN_POINT('Ctrl Pts',(0.132280018312676,-0.050595007513092,
0.24));
#19059=CARTESIAN_POINT('Ctrl Pts',(0.129952822193542,-0.0574290655609092,
0.24));
#19060=CARTESIAN_POINT('Ctrl Pts',(0.128850070284018,-0.0606674134165377,
0.24));
#19061=CARTESIAN_POINT('Ctrl Pts',(0.127623182384127,-0.0638741644409745,
0.24));
#19062=CARTESIAN_POINT('Ctrl Pts',(0.126284110088584,-0.067028198101918,
0.24));
#19063=CARTESIAN_POINT('Ctrl Pts',(0.122654675969015,-0.0755769205431157,
0.24));
#19064=CARTESIAN_POINT('Ctrl Pts',(0.118195290975453,-0.0837663478860722,
0.24));
#19065=CARTESIAN_POINT('Ctrl Pts',(0.113014989178579,-0.0915013065162071,
0.24));
#19066=CARTESIAN_POINT('Ctrl Pts',(0.108985931714537,-0.0975172866704144,
0.24));
#19067=CARTESIAN_POINT('Ctrl Pts',(0.104519884911976,-0.103258562704539,
0.24));
#19068=CARTESIAN_POINT('Ctrl Pts',(0.0996546828651377,-0.108675969178894,
0.24));
#19069=CARTESIAN_POINT('Ctrl Pts',(0.0972822643803542,-0.11131765910988,
0.24));
#19070=CARTESIAN_POINT('Ctrl Pts',(0.09482095240722,-0.113875293456495,
0.24));
#19071=CARTESIAN_POINT('Ctrl Pts',(0.0922773332174137,-0.116342466058553,
0.24));
#19072=CARTESIAN_POINT('Ctrl Pts',(0.0868426048671788,-0.121613857680014,
0.24));
#19073=CARTESIAN_POINT('Ctrl Pts',(0.0810310485854155,-0.126474759557936,
0.24));
#19074=CARTESIAN_POINT('Ctrl Pts',(0.0748870600798396,-0.130870957562724,
0.24));
#19075=CARTESIAN_POINT('Ctrl Pts',(0.0715378781224404,-0.133267392228159,
0.24));
#19076=CARTESIAN_POINT('Ctrl Pts',(0.0680912231566627,-0.135524142754832,
0.24));
#19077=CARTESIAN_POINT('Ctrl Pts',(0.0645638484115253,-0.13762659390894,
0.24));
#19078=CARTESIAN_POINT('Ctrl Pts',(0.0598451535113139,-0.140439117742,0.24));
#19079=CARTESIAN_POINT('Ctrl Pts',(0.0549775790306604,-0.142978967531553,
0.24));
#19080=CARTESIAN_POINT('Ctrl Pts',(0.0499773507040556,-0.145225083935062,
0.24));
#19081=CARTESIAN_POINT('Ctrl Pts',(0.0466920976074369,-0.146700828718701,
0.24));
#19082=CARTESIAN_POINT('Ctrl Pts',(0.0433495270099635,-0.148049731670784,
0.24));
#19083=CARTESIAN_POINT('Ctrl Pts',(0.039956549802796,-0.149273502906639,
0.24));
#19084=CARTESIAN_POINT('Ctrl Pts',(-0.126296536029262,-6.10717992316628E-5,
0.159341967361942));
#19085=CARTESIAN_POINT('Ctrl Pts',(-0.12637083907321,-0.0163056929409037,
0.160361391877968));
#19086=CARTESIAN_POINT('Ctrl Pts',(-0.12344809088261,-0.0325245895549842,
0.161380816393994));
#19087=CARTESIAN_POINT('Ctrl Pts',(-0.117399968681154,-0.0474794518833934,
0.162400240910021));
#19088=CARTESIAN_POINT('Ctrl Pts',(-0.102053636235694,-0.0854254922118417,
0.164986899546353));
#19089=CARTESIAN_POINT('Ctrl Pts',(-0.0665853528586453,-0.115233359066084,
0.167573558182686));
#19090=CARTESIAN_POINT('Ctrl Pts',(-0.0265641275910804,-0.123819689910512,
0.170160216819019));
#19091=CARTESIAN_POINT('Ctrl Pts',(0.0134570976764845,-0.13240602075494,
0.172746875455351));
#19092=CARTESIAN_POINT('Ctrl Pts',(0.058031264834566,-0.119770815589554,
0.175333534091684));
#19093=CARTESIAN_POINT('Ctrl Pts',(0.0875924985281064,-0.0914586003428122,
0.177920192728017));
#19094=CARTESIAN_POINT('Ctrl Pts',(0.117153732221647,-0.0631463850960709,
0.180506851364349));
#19095=CARTESIAN_POINT('Ctrl Pts',(0.131702032450646,-0.0191571597679751,
0.183093510000682));
#19096=CARTESIAN_POINT('Ctrl Pts',(0.124851119980295,0.0211965060081854,
0.185680168637015));
#19097=CARTESIAN_POINT('Ctrl Pts',(0.118000207509943,0.0615501717843459,
0.188266827273347));
#19098=CARTESIAN_POINT('Ctrl Pts',(0.0897500823402403,0.0982682780085711,
0.19085348590968));
#19099=CARTESIAN_POINT('Ctrl Pts',(0.0525017161220023,0.115239608835997,
0.193440144546013));
#19100=CARTESIAN_POINT('Ctrl Pts',(0.0152533499037644,0.132210939663423,
0.196026803182345));
#19101=CARTESIAN_POINT('Ctrl Pts',(-0.030993257363009,0.129435495094051,
0.198613461818678));
#19102=CARTESIAN_POINT('Ctrl Pts',(-0.0659388717692058,0.108119484364762,
0.20120012045501));
#19103=CARTESIAN_POINT('Ctrl Pts',(-0.100884486175403,0.0868034736354726,
0.203786779091343));
#19104=CARTESIAN_POINT('Ctrl Pts',(-0.124529107721023,0.0469468967462671,
0.206373437727676));
#19105=CARTESIAN_POINT('Ctrl Pts',(-0.126492123469331,0.00606801008988057,
0.208960096364008));
#19106=CARTESIAN_POINT('Ctrl Pts',(-0.126588724127832,0.00405634646811867,
0.209087386696653));
#19107=CARTESIAN_POINT('Ctrl Pts',(-0.126632819376787,0.00204220716288977,
0.209214677029297));
#19108=CARTESIAN_POINT('Ctrl Pts',(-0.126625441102054,2.7778768752873E-5,
0.209341967361942));
#19109=CARTESIAN_POINT('Ctrl Pts',(-0.0398513841857245,-0.149064942821851,
0.24));
#19110=CARTESIAN_POINT('Ctrl Pts',(-0.0883048112969314,-0.136111285829332,
0.237413341363667));
#19111=CARTESIAN_POINT('Ctrl Pts',(-0.170871437255804,-0.0596187094618861,
0.232240024091002));
#19112=CARTESIAN_POINT('Ctrl Pts',(-0.145169204726118,0.108307533342445,
0.224480048182004));
#19113=CARTESIAN_POINT('Ctrl Pts',(0.00818767200092134,0.180778621679153,
0.216720072273006));
#19114=CARTESIAN_POINT('Ctrl Pts',(0.154249898498561,0.0947283641859207,
0.208960096364008));
#19115=CARTESIAN_POINT('Ctrl Pts',(0.164950538597243,-0.0745810526211722,
0.201200120455011));
#19116=CARTESIAN_POINT('Ctrl Pts',(0.0308106631569891,-0.178364693496558,
0.193440144546012));
#19117=CARTESIAN_POINT('Ctrl Pts',(-0.13036283225522,-0.125587074703769,
0.185680168637015));
#19118=CARTESIAN_POINT('Ctrl Pts',(-0.17709781441264,0.03745832727601,0.177920192728017));
#19119=CARTESIAN_POINT('Ctrl Pts',(-0.0683530255288039,0.167611467503216,
0.170160216819019));
#19120=CARTESIAN_POINT('Ctrl Pts',(0.100397202365132,0.150621028353064,
0.162400240910021));
#19121=CARTESIAN_POINT('Ctrl Pts',(0.18100910679194,0.00139719974911195,
0.154640265001023));
#19122=CARTESIAN_POINT('Ctrl Pts',(0.102711092909207,-0.149052183789333,
0.146880289092025));
#19123=CARTESIAN_POINT('Ctrl Pts',(-0.0657574679958034,-0.168648048308422,
0.139120313183027));
#19124=CARTESIAN_POINT('Ctrl Pts',(-0.176497206835689,-0.0401861834345609,
0.131360337274029));
#19125=CARTESIAN_POINT('Ctrl Pts',(-0.132288575936487,0.123555290563421,
0.123600361365031));
#19126=CARTESIAN_POINT('Ctrl Pts',(0.0280571680938306,0.178826694862324,
0.115840385456033));
#19127=CARTESIAN_POINT('Ctrl Pts',(0.163771354656592,0.0771047007047774,
0.108080409547035));
#19128=CARTESIAN_POINT('Ctrl Pts',(0.155709331479018,-0.0923080778690166,
0.100320433638038));
#19129=CARTESIAN_POINT('Ctrl Pts',(0.0109489686262093,-0.180682908560435,
0.0925604577290397));
#19130=CARTESIAN_POINT('Ctrl Pts',(-0.143423754439364,-0.110434756566834,
0.0848004818200417));
#19131=CARTESIAN_POINT('Ctrl Pts',(-0.17188331593326,0.0567648465404429,
0.0770405059110439));
#19132=CARTESIAN_POINT('Ctrl Pts',(-0.0494457976037486,0.174130301808973,
0.0692805300020459));
#19133=CARTESIAN_POINT('Ctrl Pts',(0.11640175885633,0.13862511662766,0.061520554093048));
#19134=CARTESIAN_POINT('Ctrl Pts',(0.18005704388064,-0.0185795878987759,
0.0537605781840501));
#19135=CARTESIAN_POINT('Ctrl Pts',(0.0856431484406112,-0.159474177462153,
0.0460006022750521));
#19136=CARTESIAN_POINT('Ctrl Pts',(-0.0839657292871194,-0.160363143120653,
0.0382406263660544));
#19137=CARTESIAN_POINT('Ctrl Pts',(-0.179844832231877,-0.0204718628801216,
0.0304806504570563));
#19138=CARTESIAN_POINT('Ctrl Pts',(-0.117866479118068,0.137399078213474,
0.0227206745480585));
#19139=CARTESIAN_POINT('Ctrl Pts',(0.0476444145610997,0.174632482457551,
0.0149606986390605));
#19140=CARTESIAN_POINT('Ctrl Pts',(0.171219786572432,0.0585809927800803,
0.00720072273006264));
#19141=CARTESIAN_POINT('Ctrl Pts',(0.144688050375066,-0.108949473877577,
-0.000559253178935319));
#19142=CARTESIAN_POINT('Ctrl Pts',(-0.0092814439579932,-0.180735423716049,
-0.00831922908793317));
#19143=CARTESIAN_POINT('Ctrl Pts',(-0.105867686800049,-0.122947365648507,
-0.0134925463605985));
#19144=CARTESIAN_POINT('Ctrl Pts',(-0.131895903200816,-0.0800747195988904,
-0.0160792049969312));
#19145=CARTESIAN_POINT('Ctrl Pts',(-0.0374537582415196,-0.140096572423086,
0.245359734998977));
#19146=CARTESIAN_POINT('Ctrl Pts',(-0.0829920245295529,-0.127922261611689,
0.242773076362644));
#19147=CARTESIAN_POINT('Ctrl Pts',(-0.160591096949962,-0.0560317985556137,
0.237599759089979));
#19148=CARTESIAN_POINT('Ctrl Pts',(-0.13643521822445,0.101791299158848,
0.229839783180981));
#19149=CARTESIAN_POINT('Ctrl Pts',(0.00769506740980954,0.1699022237233,
0.222079807271983));
#19150=CARTESIAN_POINT('Ctrl Pts',(0.144969579481095,0.0890291096113304,
0.214319831362985));
#19151=CARTESIAN_POINT('Ctrl Pts',(0.155026424317845,-0.0700939445729984,
0.206559855453987));
#19152=CARTESIAN_POINT('Ctrl Pts',(0.0289569648011409,-0.167633527556011,
0.19879987954499));
#19153=CARTESIAN_POINT('Ctrl Pts',(-0.122519659046519,-0.118031231043151,
0.191039903635991));
#19154=CARTESIAN_POINT('Ctrl Pts',(-0.166442869216287,0.0352046776440443,
0.183279927726994));
#19155=CARTESIAN_POINT('Ctrl Pts',(-0.064240621638164,0.157527260611955,
0.175519951817996));
#19156=CARTESIAN_POINT('Ctrl Pts',(0.0943568867767351,0.141559037340679,
0.167759975908998));
#19157=CARTESIAN_POINT('Ctrl Pts',(0.170118841887737,0.00131313836865665,
0.16));
#19158=CARTESIAN_POINT('Ctrl Pts',(0.0965315639882279,-0.140084581027326,
0.152240024091002));
#19159=CARTESIAN_POINT('Ctrl Pts',(-0.0618012237018238,-0.158501476380598,
0.144480048182004));
#19160=CARTESIAN_POINT('Ctrl Pts',(-0.165878396703103,-0.0377684145673052,
0.136720072273006));
#19161=CARTESIAN_POINT('Ctrl Pts',(-0.124329541933827,0.116121687534276,
0.128960096364008));
#19162=CARTESIAN_POINT('Ctrl Pts',(0.0263691315170036,0.168067732987372,
0.12120012045501));
#19163=CARTESIAN_POINT('Ctrl Pts',(0.153918185014798,0.0724657594331675,
0.113440144546012));
#19164=CARTESIAN_POINT('Ctrl Pts',(0.146341206869619,-0.0867544378416841,
0.105680168637015));
#19165=CARTESIAN_POINT('Ctrl Pts',(0.0102902328814698,-0.169812269106107,
0.0979201927280167));
#19166=CARTESIAN_POINT('Ctrl Pts',(-0.134794781526993,-0.103790539737311,
0.0901602168190187));
#19167=CARTESIAN_POINT('Ctrl Pts',(-0.161542096774173,0.0533496359633175,
0.0824002409100209));
#19168=CARTESIAN_POINT('Ctrl Pts',(-0.0464709316213242,0.163653894581969,
0.074640265001023));
#19169=CARTESIAN_POINT('Ctrl Pts',(0.109398542213106,0.130284849835523,
0.066880289092025));
#19170=CARTESIAN_POINT('Ctrl Pts',(0.16922405906302,-0.0174617621848401,
0.0591203131830272));
#19171=CARTESIAN_POINT('Ctrl Pts',(0.0804904984426183,-0.149879543972585,
0.0513603372740291));
#19172=CARTESIAN_POINT('Ctrl Pts',(-0.0789139998409189,-0.150715025739123,
0.0436003613650314));
#19173=CARTESIAN_POINT('Ctrl Pts',(-0.169024614954586,-0.0192401899891918,
0.0358403854560333));
#19174=CARTESIAN_POINT('Ctrl Pts',(-0.110775138777956,0.12913257502003,
0.0280804095470356));
#19175=CARTESIAN_POINT('Ctrl Pts',(0.0447779273164969,0.164125861942445,
0.0203204336380375));
#19176=CARTESIAN_POINT('Ctrl Pts',(0.16091848811479,0.0550565152494576,
0.0125604577290397));
#19177=CARTESIAN_POINT('Ctrl Pts',(0.135983012131502,-0.10239461786658,
0.00480048182004171));
#19178=CARTESIAN_POINT('Ctrl Pts',(-0.00872303347143,-0.169861624730324,
-0.00295949408895612));
#19179=CARTESIAN_POINT('Ctrl Pts',(-0.0994982439886826,-0.115550337924785,
-0.00813281136162148));
#19180=CARTESIAN_POINT('Ctrl Pts',(-0.123960494032221,-0.0752570895690155,
-0.0107194699979541));
#19181=CARTESIAN_POINT('Ctrl Pts',(-0.0350561322973148,-0.13112820202432,
0.250719469997954));
#19182=CARTESIAN_POINT('Ctrl Pts',(-0.0776792377621743,-0.119733237394047,
0.248132811361621));
#19183=CARTESIAN_POINT('Ctrl Pts',(-0.150310756644121,-0.0524448876493412,
0.242959494088956));
#19184=CARTESIAN_POINT('Ctrl Pts',(-0.127701231722781,0.0952750649752511,
0.235199518179958));
#19185=CARTESIAN_POINT('Ctrl Pts',(0.00720246281869772,0.159025825767447,
0.22743954227096));
#19186=CARTESIAN_POINT('Ctrl Pts',(0.135689260463629,0.08332985503674,0.219679566361962));
#19187=CARTESIAN_POINT('Ctrl Pts',(0.145102310038447,-0.0656068365248246,
0.211919590452964));
#19188=CARTESIAN_POINT('Ctrl Pts',(0.0271032664452926,-0.156902361615465,
0.204159614543967));
#19189=CARTESIAN_POINT('Ctrl Pts',(-0.114676485837817,-0.110475387382534,
0.196399638634969));
#19190=CARTESIAN_POINT('Ctrl Pts',(-0.155787924019933,0.0329510280120788,
0.188639662725971));
#19191=CARTESIAN_POINT('Ctrl Pts',(-0.0601282177475243,0.147443053720694,
0.180879686816973));
#19192=CARTESIAN_POINT('Ctrl Pts',(0.0883165711883383,0.132497046328295,
0.173119710907975));
#19193=CARTESIAN_POINT('Ctrl Pts',(0.159228576983534,0.00122907698820117,
0.165359734998977));
#19194=CARTESIAN_POINT('Ctrl Pts',(0.0903520350672485,-0.131116978265319,
0.157599759089979));
#19195=CARTESIAN_POINT('Ctrl Pts',(-0.0578449794078444,-0.148354904452775,
0.149839783180981));
#19196=CARTESIAN_POINT('Ctrl Pts',(-0.155259586570517,-0.0353506457000499,
0.142079807271983));
#19197=CARTESIAN_POINT('Ctrl Pts',(-0.116370507931168,0.108688084505131,
0.134319831362985));
#19198=CARTESIAN_POINT('Ctrl Pts',(0.0246810949401768,0.157308771112418,
0.126559855453988));
#19199=CARTESIAN_POINT('Ctrl Pts',(0.144065015373005,0.0678268181615582,
0.118799879544989));
#19200=CARTESIAN_POINT('Ctrl Pts',(0.13697308226022,-0.0812007978143519,
0.111039903635992));
#19201=CARTESIAN_POINT('Ctrl Pts',(0.00963149713673027,-0.15894162965178,
0.103279927726994));
#19202=CARTESIAN_POINT('Ctrl Pts',(-0.126165808614623,-0.0971463229077874,
0.0955199518179957));
#19203=CARTESIAN_POINT('Ctrl Pts',(-0.151200877615086,0.0499344253861922,
0.087759975908998));
#19204=CARTESIAN_POINT('Ctrl Pts',(-0.0434960656388994,0.153177487354966,
0.08));
#19205=CARTESIAN_POINT('Ctrl Pts',(0.102395325569881,0.121944583043386,
0.072240024091002));
#19206=CARTESIAN_POINT('Ctrl Pts',(0.158391074245402,-0.0163439364709043,
0.0644800481820042));
#19207=CARTESIAN_POINT('Ctrl Pts',(0.0753378484446251,-0.140284910483017,
0.0567200722730062));
#19208=CARTESIAN_POINT('Ctrl Pts',(-0.0738622703947183,-0.141066908357593,
0.0489600963640083));
#19209=CARTESIAN_POINT('Ctrl Pts',(-0.158204397677296,-0.018008517098262,
0.0412001204550104));
#19210=CARTESIAN_POINT('Ctrl Pts',(-0.103683798437843,0.120866071826586,
0.0334401445460125));
#19211=CARTESIAN_POINT('Ctrl Pts',(0.0419114400718942,0.153619241427338,
0.0256801686370146));
#19212=CARTESIAN_POINT('Ctrl Pts',(0.150617189657149,0.051532037718835,
0.0179201927280167));
#19213=CARTESIAN_POINT('Ctrl Pts',(0.127277973887939,-0.0958397618555833,
0.0101602168190187));
#19214=CARTESIAN_POINT('Ctrl Pts',(-0.00816462298486686,-0.1589878257446,
0.00240024091002091));
#19215=CARTESIAN_POINT('Ctrl Pts',(-0.0931288011773165,-0.108153310201063,
-0.00277307636264444));
#19216=CARTESIAN_POINT('Ctrl Pts',(-0.116025084863626,-0.0704394595391406,
-0.00535973499897709));
#19217=CARTESIAN_POINT('Ctrl Pts',(-0.0326585063531099,-0.122159831625555,
0.256079204996931));
#19218=CARTESIAN_POINT('Ctrl Pts',(-0.0723664509947957,-0.111544213176404,
0.253492546360598));
#19219=CARTESIAN_POINT('Ctrl Pts',(-0.140030416338279,-0.0488579767430688,
0.248319229087933));
#19220=CARTESIAN_POINT('Ctrl Pts',(-0.118967245221113,0.0887588307916541,
0.240559253178936));
#19221=CARTESIAN_POINT('Ctrl Pts',(0.00670985822758596,0.148149427811594,
0.232799277269937));
#19222=CARTESIAN_POINT('Ctrl Pts',(0.126408941446163,0.0776306004621497,
0.225039301360939));
#19223=CARTESIAN_POINT('Ctrl Pts',(0.13517819575905,-0.0611197284766509,
0.217279325451942));
#19224=CARTESIAN_POINT('Ctrl Pts',(0.0252495680894444,-0.146171195674918,
0.209519349542944));
#19225=CARTESIAN_POINT('Ctrl Pts',(-0.106833312629116,-0.102919543721916,
0.201759373633946));
#19226=CARTESIAN_POINT('Ctrl Pts',(-0.14513297882358,0.0306973783801131,
0.193999397724948));
#19227=CARTESIAN_POINT('Ctrl Pts',(-0.0560158138568844,0.137358846829434,
0.18623942181595));
#19228=CARTESIAN_POINT('Ctrl Pts',(0.0822762555999414,0.12343505531591,
0.178479445906952));
#19229=CARTESIAN_POINT('Ctrl Pts',(0.148338312079331,0.00114501560774606,
0.170719469997954));
#19230=CARTESIAN_POINT('Ctrl Pts',(0.0841725061462688,-0.122149375503312,
0.162959494088956));
#19231=CARTESIAN_POINT('Ctrl Pts',(-0.0538887351138648,-0.138208332524951,
0.155199518179959));
#19232=CARTESIAN_POINT('Ctrl Pts',(-0.144640776437932,-0.0329328768327946,
0.14743954227096));
#19233=CARTESIAN_POINT('Ctrl Pts',(-0.108411473928508,0.101254481475986,
0.139679566361963));
#19234=CARTESIAN_POINT('Ctrl Pts',(0.0229930583633497,0.146549809237466,
0.131919590452964));
#19235=CARTESIAN_POINT('Ctrl Pts',(0.134211845731212,0.0631878768899486,
0.124159614543967));
#19236=CARTESIAN_POINT('Ctrl Pts',(0.127604957650822,-0.0756471577870196,
0.116399638634969));
#19237=CARTESIAN_POINT('Ctrl Pts',(0.00897276139199077,-0.148070990197453,
0.108639662725971));
#19238=CARTESIAN_POINT('Ctrl Pts',(-0.117536835702253,-0.0905021060782641,
0.100879686816973));
#19239=CARTESIAN_POINT('Ctrl Pts',(-0.140859658455999,0.0465192148090667,
0.0931197109079749));
#19240=CARTESIAN_POINT('Ctrl Pts',(-0.0405211996564747,0.142701080127962,
0.0853597349989771));
#19241=CARTESIAN_POINT('Ctrl Pts',(0.0953921089266558,0.113604316251249,
0.077599759089979));
#19242=CARTESIAN_POINT('Ctrl Pts',(0.147558089427783,-0.0152261107569683,
0.0698397831809813));
#19243=CARTESIAN_POINT('Ctrl Pts',(0.070185198446632,-0.130690276993449,
0.0620798072719832));
#19244=CARTESIAN_POINT('Ctrl Pts',(-0.0688105409485176,-0.131418790976063,
0.0543198313629854));
#19245=CARTESIAN_POINT('Ctrl Pts',(-0.147384180400005,-0.0167768442073323,
0.0465598554539874));
#19246=CARTESIAN_POINT('Ctrl Pts',(-0.0965924580977301,0.112599568633142,
0.0387998795449896));
#19247=CARTESIAN_POINT('Ctrl Pts',(0.0390449528272914,0.143112620912232,
0.0310399036359916));
#19248=CARTESIAN_POINT('Ctrl Pts',(0.140315891199508,0.0480075601882123,
0.0232799277269937));
#19249=CARTESIAN_POINT('Ctrl Pts',(0.118572935644375,-0.0892849058445864,
0.0155199518179958));
#19250=CARTESIAN_POINT('Ctrl Pts',(-0.00760621249830358,-0.148114026758875,
0.00775997590899793));
#19251=CARTESIAN_POINT('Ctrl Pts',(-0.0867593583659504,-0.100756282477341,
0.00258665863633259));
#19252=CARTESIAN_POINT('Ctrl Pts',(-0.108089675695031,-0.0656218295092657,
-5.55111512312578E-17));
#19253=CARTESIAN_POINT('Ctrl Pts',(-0.108089675695031,-0.0656218295092657,
-5.55111512312578E-17));
#19254=CARTESIAN_POINT('Ctrl Pts',(-0.104219465379748,-0.0739058869203245,
-4.02841154597017E-17));
#19255=CARTESIAN_POINT('Ctrl Pts',(-0.0994141168358061,-0.0816768736924768,
-5.16144647363644E-17));
#19256=CARTESIAN_POINT('Ctrl Pts',(-0.0938412360364922,-0.088871564406415,
-3.81639164714898E-17));
#19257=CARTESIAN_POINT('Ctrl Pts',(-0.0894001862863345,-0.094605040600905,
-2.74451237748006E-17));
#19258=CARTESIAN_POINT('Ctrl Pts',(-0.0844703330957707,-0.0999727304469881,
3.12377098840079E-17));
#19259=CARTESIAN_POINT('Ctrl Pts',(-0.0791158513129458,-0.104935071387697,
-1.21430643318376E-17));
#19260=CARTESIAN_POINT('Ctrl Pts',(-0.0766900604813501,-0.107183206995485,
-3.17962611543325E-17));
#19261=CARTESIAN_POINT('Ctrl Pts',(-0.0741829996358932,-0.109342173006691,
4.83248416902999E-17));
#19262=CARTESIAN_POINT('Ctrl Pts',(-0.0716059924168524,-0.111405381598006,
5.3776427755281E-17));
#19263=CARTESIAN_POINT('Ctrl Pts',(-0.0639212992135713,-0.117557915794061,
7.00331794132204E-17));
#19264=CARTESIAN_POINT('Ctrl Pts',(-0.0556061968393146,-0.12287204611112,
-5.69073736333764E-18));
#19265=CARTESIAN_POINT('Ctrl Pts',(-0.0468203466856493,-0.127256781127915,
5.55111512312578E-17));
#19266=CARTESIAN_POINT('Ctrl Pts',(-0.0434613267337519,-0.12893315986732,
7.89099528597243E-17));
#19267=CARTESIAN_POINT('Ctrl Pts',(-0.0400330653128497,-0.130473352587733,
3.97002991909352E-17));
#19268=CARTESIAN_POINT('Ctrl Pts',(-0.0365431560942257,-0.131870761756357,
6.59194920871187E-17));
#19269=CARTESIAN_POINT('Ctrl Pts',(-0.0339571636773035,-0.13290622981212,
8.5347686277821E-17));
#19270=CARTESIAN_POINT('Ctrl Pts',(-0.0313383144727484,-0.133862652235137,
-2.74403076010104E-17));
#19271=CARTESIAN_POINT('Ctrl Pts',(-0.0286994266230122,-0.134734580282325,
-2.42861286636753E-17));
#19272=CARTESIAN_POINT('Ctrl Pts',(-0.0216199050576346,-0.137073760181214,
-1.58242011095522E-17));
#19273=CARTESIAN_POINT('Ctrl Pts',(-0.0143790427459088,-0.138813119073991,
5.80198461902811E-17));
#19274=CARTESIAN_POINT('Ctrl Pts',(-0.0070411538297537,-0.139912507657099,
6.93889390390723E-17));
#19275=CARTESIAN_POINT('Ctrl Pts',(5.47883476400097E-5,-0.140975646920361,
8.02325614020808E-17));
#19276=CARTESIAN_POINT('Ctrl Pts',(0.00724182591717642,-0.141440539972256,
1.32011341321413E-16));
#19277=CARTESIAN_POINT('Ctrl Pts',(0.0144605478337719,-0.141339082434075,
1.61329283265843E-16));
#19278=CARTESIAN_POINT('Ctrl Pts',(0.0178811722145177,-0.141291006315792,
1.75221724083914E-16));
#19279=CARTESIAN_POINT('Ctrl Pts',(0.021310106848269,-0.141115105569205,
1.85534911235541E-16));
#19280=CARTESIAN_POINT('Ctrl Pts',(0.0247235715439624,-0.140816220288761,
1.71737624121704E-16));
#19281=CARTESIAN_POINT('Ctrl Pts',(0.0339754553361668,-0.140006119078294,
1.34341339582434E-16));
#19282=CARTESIAN_POINT('Ctrl Pts',(0.0431421008898472,-0.138295657968001,
8.04496487960062E-17));
#19283=CARTESIAN_POINT('Ctrl Pts',(0.0520992976556894,-0.135759125106636,
3.20923843055709E-17));
#19284=CARTESIAN_POINT('Ctrl Pts',(0.0590658916121619,-0.13378629867842,
-5.518202506064E-18));
#19285=CARTESIAN_POINT('Ctrl Pts',(0.0659062642374416,-0.131312982137409,
7.87850579480063E-17));
#19286=CARTESIAN_POINT('Ctrl Pts',(0.0725619642951071,-0.128359965266718,
7.63278329429795E-17));
#19287=CARTESIAN_POINT('Ctrl Pts',(0.0758074813473741,-0.126919986522721,
7.51296170399226E-17));
#19288=CARTESIAN_POINT('Ctrl Pts',(0.0790005264283722,-0.125369490597537,
8.38688896655138E-17));
#19289=CARTESIAN_POINT('Ctrl Pts',(0.0821329715644795,-0.123712761836801,
7.24247051220317E-17));
#19290=CARTESIAN_POINT('Ctrl Pts',(0.0888257654942848,-0.120172989003949,
4.79730178566093E-17));
#19291=CARTESIAN_POINT('Ctrl Pts',(0.0952446087626691,-0.116147988031934,
8.96774285244103E-17));
#19292=CARTESIAN_POINT('Ctrl Pts',(0.101324221742587,-0.111663228753314,
8.28330459778925E-17));
#19293=CARTESIAN_POINT('Ctrl Pts',(0.104638321741973,-0.109218510516871,
7.91020571356516E-17));
#19294=CARTESIAN_POINT('Ctrl Pts',(0.107849695272814,-0.106637925639498,
3.17151869302413E-17));
#19295=CARTESIAN_POINT('Ctrl Pts',(0.110939265073957,-0.10393289123317,
1.53956708492942E-17));
#19296=CARTESIAN_POINT('Ctrl Pts',(0.115072333360666,-0.100314234708527,
-6.43574216607592E-18));
#19297=CARTESIAN_POINT('Ctrl Pts',(0.118992075260627,-0.0964697210975667,
5.54296751400654E-17));
#19298=CARTESIAN_POINT('Ctrl Pts',(0.122673447199167,-0.0924082746861152,
3.52365706057789E-17));
#19299=CARTESIAN_POINT('Ctrl Pts',(0.125092164655522,-0.0897398425098966,
2.31620156359627E-17));
#19300=CARTESIAN_POINT('Ctrl Pts',(0.127407959881093,-0.0869777021544565,
-4.01489640485901E-17));
#19301=CARTESIAN_POINT('Ctrl Pts',(0.129620323775263,-0.0841289546921697,
-3.98986399474666E-17));
#19302=CARTESIAN_POINT('Ctrl Pts',(-0.126471935391749,0.000101176582396995,
0.195658032638058));
#19303=CARTESIAN_POINT('Ctrl Pts',(-0.126547267107008,0.00888033934128026,
0.195105154333688));
#19304=CARTESIAN_POINT('Ctrl Pts',(-0.125707148272093,0.0176451944231377,
0.194552276029318));
#19305=CARTESIAN_POINT('Ctrl Pts',(-0.12389684029672,0.0262048027713284,
0.193999397724948));
#19306=CARTESIAN_POINT('Ctrl Pts',(-0.115427257168015,0.0662512011965534,
0.191412739088615));
#19307=CARTESIAN_POINT('Ctrl Pts',(-0.0857215355124495,0.101805024012994,
0.188826080452282));
#19308=CARTESIAN_POINT('Ctrl Pts',(-0.0478199964418627,0.117261303502293,
0.18623942181595));
#19309=CARTESIAN_POINT('Ctrl Pts',(-0.0099184573712758,0.132717582991593,
0.183652763179617));
#19310=CARTESIAN_POINT('Ctrl Pts',(0.0361788991143328,0.128076319153751,
0.181066104543285));
#19311=CARTESIAN_POINT('Ctrl Pts',(0.070237920103702,0.105374013950137,
0.178479445906952));
#19312=CARTESIAN_POINT('Ctrl Pts',(0.104296941093071,0.0826717087465222,
0.175892787270619));
#19313=CARTESIAN_POINT('Ctrl Pts',(0.126317626586201,0.0419083621771342,
0.173306128634287));
#19314=CARTESIAN_POINT('Ctrl Pts',(0.126633668343922,0.000977623707263797,
0.170719469997954));
#19315=CARTESIAN_POINT('Ctrl Pts',(0.126949710101644,-0.0399531147626067,
0.168132811361621));
#19316=CARTESIAN_POINT('Ctrl Pts',(0.105561108123956,-0.08105124513296,
0.165546152725289));
#19317=CARTESIAN_POINT('Ctrl Pts',(0.0718566002584231,-0.104276803155076,
0.162959494088956));
#19318=CARTESIAN_POINT('Ctrl Pts',(0.0381520923928904,-0.127502361177192,
0.160372835452623));
#19319=CARTESIAN_POINT('Ctrl Pts',(-0.00786832136048696,-0.132855346851071,
0.157786176816291));
#19320=CARTESIAN_POINT('Ctrl Pts',(-0.0460038684578537,-0.117985930405985,
0.155199518179958));
#19321=CARTESIAN_POINT('Ctrl Pts',(-0.0841394155552204,-0.103116513960899,
0.152612859543626));
#19322=CARTESIAN_POINT('Ctrl Pts',(-0.114390095996576,-0.0680246953968468,
0.150026200907293));
#19323=CARTESIAN_POINT('Ctrl Pts',(-0.12347721913235,-0.0281142263966907,
0.14743954227096));
#19324=CARTESIAN_POINT('Ctrl Pts',(-0.125563410841138,-0.018951712774069,
0.14684570572666));
#19325=CARTESIAN_POINT('Ctrl Pts',(-0.126534167537385,-0.00953522996602069,
0.146251869182359));
#19326=CARTESIAN_POINT('Ctrl Pts',(-0.126453631260982,-0.000102348163238207,
0.145658032638058));
#19327=CARTESIAN_POINT('Ctrl Pts',(-0.0398513841857245,-0.149064942821851,
0.24));
#19328=CARTESIAN_POINT('Ctrl Pts',(-0.0498806325786677,-0.145400296738327,
0.24));
#19329=CARTESIAN_POINT('Ctrl Pts',(-0.0594363948008725,-0.140639648297949,
0.24));
#19330=CARTESIAN_POINT('Ctrl Pts',(-0.0684062055177017,-0.134931499399492,
0.24));
#19331=CARTESIAN_POINT('Ctrl Pts',(-0.0735915624001909,-0.131631676235849,
0.24));
#19332=CARTESIAN_POINT('Ctrl Pts',(-0.0785806353345173,-0.128014298080738,
0.24));
#19333=CARTESIAN_POINT('Ctrl Pts',(-0.0833462611484583,-0.124102693747304,
0.24));
#19334=CARTESIAN_POINT('Ctrl Pts',(-0.0858656342542594,-0.122034803580736,
0.24));
#19335=CARTESIAN_POINT('Ctrl Pts',(-0.0883241156266364,-0.11988309220465,
0.24));
#19336=CARTESIAN_POINT('Ctrl Pts',(-0.0907117892851122,-0.117655751751618,
0.24));
#19337=CARTESIAN_POINT('Ctrl Pts',(-0.0983819858496404,-0.110500611839494,
0.24));
#19338=CARTESIAN_POINT('Ctrl Pts',(-0.105284458416918,-0.102606966330569,
0.24));
#19339=CARTESIAN_POINT('Ctrl Pts',(-0.111294422020379,-0.0941015332659665,
0.24));
#19340=CARTESIAN_POINT('Ctrl Pts',(-0.114410577497229,-0.0896914812962706,
0.24));
#19341=CARTESIAN_POINT('Ctrl Pts',(-0.117286101138547,-0.0851164738413172,
0.24));
#19342=CARTESIAN_POINT('Ctrl Pts',(-0.119898298320422,-0.0803922539627851,
0.24));
#19343=CARTESIAN_POINT('Ctrl Pts',(-0.1222721977331,-0.0760990011896685,
0.24));
#19344=CARTESIAN_POINT('Ctrl Pts',(-0.124430744329062,-0.0716759619599862,
0.24));
#19345=CARTESIAN_POINT('Ctrl Pts',(-0.126341093034125,-0.0671690272221462,
0.24));
#19346=CARTESIAN_POINT('Ctrl Pts',(-0.129206708925078,-0.060408406100978,
0.24));
#19347=CARTESIAN_POINT('Ctrl Pts',(-0.131522065955468,-0.0534490321795157,
0.24));
#19348=CARTESIAN_POINT('Ctrl Pts',(-0.133233091500091,-0.0463330844490581,
0.24));
#19349=CARTESIAN_POINT('Ctrl Pts',(-0.135004134506116,-0.0389675313754268,
0.24));
#19350=CARTESIAN_POINT('Ctrl Pts',(-0.136127599829873,-0.0314337185245799,
0.24));
#19351=CARTESIAN_POINT('Ctrl Pts',(-0.136615064298196,-0.0238138180582873,
0.24));
#19352=CARTESIAN_POINT('Ctrl Pts',(-0.136813484749433,-0.0207121682209076,
0.24));
#19353=CARTESIAN_POINT('Ctrl Pts',(-0.136906013213758,-0.0175970392000076,
0.24));
#19354=CARTESIAN_POINT('Ctrl Pts',(-0.136893785357156,-0.0144871321155608,
0.24));
#19355=CARTESIAN_POINT('Ctrl Pts',(-0.136861203984761,-0.00620072149302863,
0.24));
#19356=CARTESIAN_POINT('Ctrl Pts',(-0.136088646936857,0.00207357465703332,
0.24));
#19357=CARTESIAN_POINT('Ctrl Pts',(-0.134599584032292,0.0102285531249486,
0.24));
#19358=CARTESIAN_POINT('Ctrl Pts',(-0.133676409755049,0.0152843948425598,
0.24));
#19359=CARTESIAN_POINT('Ctrl Pts',(-0.132477333465274,0.0202942984003417,
0.24));
#19360=CARTESIAN_POINT('Ctrl Pts',(-0.131003622030167,0.0252303138624672,
0.24));
#19361=CARTESIAN_POINT('Ctrl Pts',(-0.129740734874544,0.029460199292259,
0.24));
#19362=CARTESIAN_POINT('Ctrl Pts',(-0.128274507607502,0.0336384499732856,
0.24));
#19363=CARTESIAN_POINT('Ctrl Pts',(-0.126614574688298,0.0377237273426867,
0.24));
#19364=CARTESIAN_POINT('Ctrl Pts',(-0.124573382985647,0.042747324485064,
0.24));
#19365=CARTESIAN_POINT('Ctrl Pts',(-0.122237651925267,0.0476379767326878,
0.24));
#19366=CARTESIAN_POINT('Ctrl Pts',(-0.119609691052418,0.0523617558795304,
0.24));
#19367=CARTESIAN_POINT('Ctrl Pts',(-0.117006563775536,0.0570408964535612,
0.24));
#19368=CARTESIAN_POINT('Ctrl Pts',(-0.114113358229268,0.0615597689541448,
0.24));
#19369=CARTESIAN_POINT('Ctrl Pts',(-0.110947628485839,0.0658586917144141,
0.24));
#19370=CARTESIAN_POINT('Ctrl Pts',(-0.108265305855902,0.0695011687224882,
0.24));
#19371=CARTESIAN_POINT('Ctrl Pts',(-0.105385772272888,0.0729892759232728,
0.24));
#19372=CARTESIAN_POINT('Ctrl Pts',(-0.102309360287629,0.0763011815833395,
0.24));
#19373=CARTESIAN_POINT('Ctrl Pts',(-0.100282916666232,0.0784827457339379,
0.24));
#19374=CARTESIAN_POINT('Ctrl Pts',(-0.0981709975111385,0.0805877996091198,
0.24));
#19375=CARTESIAN_POINT('Ctrl Pts',(-0.0959791030802606,0.0826138105732947,
0.24));
#19376=CARTESIAN_POINT('Origin',(0.,0.,0.24));
#19377=CARTESIAN_POINT('',(0.158771324027147,-0.275,0.24));
#19378=CARTESIAN_POINT('',(0.317542648054294,0.,0.24));
#19379=CARTESIAN_POINT('',(0.158771324027147,-0.275,0.24));
#19380=CARTESIAN_POINT('',(0.158771324027147,0.275,0.24));
#19381=CARTESIAN_POINT('',(0.317542648054294,0.,0.24));
#19382=CARTESIAN_POINT('',(-0.158771324027147,0.275,0.24));
#19383=CARTESIAN_POINT('',(0.158771324027147,0.275,0.24));
#19384=CARTESIAN_POINT('',(-0.317542648054294,5.55111512312578E-17,0.24));
#19385=CARTESIAN_POINT('',(-0.158771324027147,0.275,0.24));
#19386=CARTESIAN_POINT('',(-0.158771324027147,-0.275,0.24));
#19387=CARTESIAN_POINT('',(-0.317542648054294,3.88877587532466E-17,0.24));
#19388=CARTESIAN_POINT('',(-0.158771324027147,-0.275,0.24));
#19389=CARTESIAN_POINT('Origin',(0.,0.,0.12));
#19390=CARTESIAN_POINT('Origin',(-0.158771324027147,-0.275,0.));
#19391=CARTESIAN_POINT('',(-0.158771324027147,-0.275,0.));
#19392=CARTESIAN_POINT('',(0.158771324027147,-0.275,0.));
#19393=CARTESIAN_POINT('',(-0.158771324027147,-0.275,0.));
#19394=CARTESIAN_POINT('',(0.158771324027147,-0.275,0.));
#19395=CARTESIAN_POINT('',(-0.158771324027147,-0.275,0.));
#19396=CARTESIAN_POINT('Origin',(-0.317542648054294,3.88877587532466E-17,
0.));
#19397=CARTESIAN_POINT('',(-0.317542648054294,3.88877587532466E-17,0.));
#19398=CARTESIAN_POINT('',(-0.317542648054294,3.88877587532466E-17,0.));
#19399=CARTESIAN_POINT('',(-0.317542648054294,3.88877587532466E-17,0.));
#19400=CARTESIAN_POINT('Origin',(-0.158771324027147,0.275,0.));
#19401=CARTESIAN_POINT('',(-0.158771324027147,0.275,0.));
#19402=CARTESIAN_POINT('',(-0.158771324027147,0.275,0.));
#19403=CARTESIAN_POINT('',(-0.158771324027147,0.275,0.));
#19404=CARTESIAN_POINT('Origin',(0.158771324027147,0.275,0.));
#19405=CARTESIAN_POINT('',(0.158771324027147,0.275,0.));
#19406=CARTESIAN_POINT('',(0.158771324027147,0.275,0.));
#19407=CARTESIAN_POINT('',(0.158771324027147,0.275,0.));
#19408=CARTESIAN_POINT('Origin',(0.317542648054294,0.,0.));
#19409=CARTESIAN_POINT('',(0.317542648054294,0.,0.));
#19410=CARTESIAN_POINT('',(0.317542648054294,0.,0.));
#19411=CARTESIAN_POINT('',(0.317542648054294,0.,0.));
#19412=CARTESIAN_POINT('Origin',(0.158771324027147,-0.275,0.));
#19413=CARTESIAN_POINT('',(0.158771324027147,-0.275,0.));
#19414=CARTESIAN_POINT('Origin',(0.,0.,0.));
#19415=CARTESIAN_POINT('',(0.,0.,0.));
#19416=CARTESIAN_POINT('',(0.,0.,0.));
#19417=CARTESIAN_POINT('',(0.,0.,0.));
#19418=CARTESIAN_POINT('',(2.,0.,0.6));
#19419=CARTESIAN_POINT('',(2.,0.,-0.84));
#19420=CARTESIAN_POINT('',(0.,0.,0.));
#19421=CARTESIAN_POINT('',(10.,0.,0.6));
#19422=CARTESIAN_POINT('',(10.,0.,-0.84));
#19423=CARTESIAN_POINT('',(0.,0.,0.));
#19424=CARTESIAN_POINT('Origin',(0.,0.,0.));
#19425=CARTESIAN_POINT('',(-0.41,-5.02105187650415E-17,0.1));
#19426=CARTESIAN_POINT('Origin',(0.,0.,0.1));
#19427=CARTESIAN_POINT('',(-0.41,-5.02105187650415E-17,0.));
#19428=CARTESIAN_POINT('',(-0.41,-5.02105187650415E-17,0.));
#19429=CARTESIAN_POINT('Origin',(0.,0.,0.));
#19430=CARTESIAN_POINT('Origin',(0.,0.,0.));
#19431=CARTESIAN_POINT('',(-0.6,-7.34788079488412E-17,0.1));
#19432=CARTESIAN_POINT('Origin',(0.,0.,0.1));
#19433=CARTESIAN_POINT('',(-0.6,-7.34788079488412E-17,0.));
#19434=CARTESIAN_POINT('',(-0.6,-7.34788079488412E-17,0.));
#19435=CARTESIAN_POINT('Origin',(0.,0.,0.));
#19436=CARTESIAN_POINT('Origin',(0.,0.,0.1));
#19437=CARTESIAN_POINT('Origin',(0.,0.,0.));
#19438=CARTESIAN_POINT('',(0.,0.,0.));
#19439=CARTESIAN_POINT('',(0.,0.,0.));
#19440=CARTESIAN_POINT('',(4.,-2.5,0.3));
#19441=CARTESIAN_POINT('',(0.,0.,0.));
#19442=CARTESIAN_POINT('',(0.,0.,0.6));
#19443=CARTESIAN_POINT('',(0.,0.,0.7));
#19444=CARTESIAN_POINT('',(4.,2.5,-0.3));
#19445=CARTESIAN_POINT('',(0.,0.,-0.7));
#19446=UNCERTAINTY_MEASURE_WITH_UNIT(LENGTH_MEASURE(0.001),#19472,
'DISTANCE_ACCURACY_VALUE',
'Maximum model space distance between geometric entities at asserted c
onnectivities');
#19447=UNCERTAINTY_MEASURE_WITH_UNIT(LENGTH_MEASURE(0.001),#19472,
'DISTANCE_ACCURACY_VALUE',
'Maximum model space distance between geometric entities at asserted c
onnectivities');
#19448=UNCERTAINTY_MEASURE_WITH_UNIT(LENGTH_MEASURE(0.001),#19472,
'DISTANCE_ACCURACY_VALUE',
'Maximum model space distance between geometric entities at asserted c
onnectivities');
#19449=UNCERTAINTY_MEASURE_WITH_UNIT(LENGTH_MEASURE(0.001),#19472,
'DISTANCE_ACCURACY_VALUE',
'Maximum model space distance between geometric entities at asserted c
onnectivities');
#19450=UNCERTAINTY_MEASURE_WITH_UNIT(LENGTH_MEASURE(0.001),#19472,
'DISTANCE_ACCURACY_VALUE',
'Maximum model space distance between geometric entities at asserted c
onnectivities');
#19451=UNCERTAINTY_MEASURE_WITH_UNIT(LENGTH_MEASURE(0.001),#19472,
'DISTANCE_ACCURACY_VALUE',
'Maximum model space distance between geometric entities at asserted c
onnectivities');
#19452=UNCERTAINTY_MEASURE_WITH_UNIT(LENGTH_MEASURE(0.001),#19472,
'DISTANCE_ACCURACY_VALUE',
'Maximum model space distance between geometric entities at asserted c
onnectivities');
#19453=UNCERTAINTY_MEASURE_WITH_UNIT(LENGTH_MEASURE(0.001),#19472,
'DISTANCE_ACCURACY_VALUE',
'Maximum model space distance between geometric entities at asserted c
onnectivities');
#19454=UNCERTAINTY_MEASURE_WITH_UNIT(LENGTH_MEASURE(0.001),#19472,
'DISTANCE_ACCURACY_VALUE',
'Maximum model space distance between geometric entities at asserted c
onnectivities');
#19455=UNCERTAINTY_MEASURE_WITH_UNIT(LENGTH_MEASURE(0.001),#19472,
'DISTANCE_ACCURACY_VALUE',
'Maximum model space distance between geometric entities at asserted c
onnectivities');
#19456=UNCERTAINTY_MEASURE_WITH_UNIT(LENGTH_MEASURE(0.001),#19472,
'DISTANCE_ACCURACY_VALUE',
'Maximum model space distance between geometric entities at asserted c
onnectivities');
#19457=UNCERTAINTY_MEASURE_WITH_UNIT(LENGTH_MEASURE(0.001),#19472,
'DISTANCE_ACCURACY_VALUE',
'Maximum model space distance between geometric entities at asserted c
onnectivities');
#19458=UNCERTAINTY_MEASURE_WITH_UNIT(LENGTH_MEASURE(0.001),#19472,
'DISTANCE_ACCURACY_VALUE',
'Maximum model space distance between geometric entities at asserted c
onnectivities');
#19459=(
GEOMETRIC_REPRESENTATION_CONTEXT(3)
GLOBAL_UNCERTAINTY_ASSIGNED_CONTEXT((#19446))
GLOBAL_UNIT_ASSIGNED_CONTEXT((#19472,#19474,#19475))
REPRESENTATION_CONTEXT('','3D')
);
#19460=(
GEOMETRIC_REPRESENTATION_CONTEXT(3)
GLOBAL_UNCERTAINTY_ASSIGNED_CONTEXT((#19447))
GLOBAL_UNIT_ASSIGNED_CONTEXT((#19472,#19474,#19475))
REPRESENTATION_CONTEXT('','3D')
);
#19461=(
GEOMETRIC_REPRESENTATION_CONTEXT(3)
GLOBAL_UNCERTAINTY_ASSIGNED_CONTEXT((#19448))
GLOBAL_UNIT_ASSIGNED_CONTEXT((#19472,#19474,#19475))
REPRESENTATION_CONTEXT('','3D')
);
#19462=(
GEOMETRIC_REPRESENTATION_CONTEXT(3)
GLOBAL_UNCERTAINTY_ASSIGNED_CONTEXT((#19449))
GLOBAL_UNIT_ASSIGNED_CONTEXT((#19472,#19474,#19475))
REPRESENTATION_CONTEXT('','3D')
);
#19463=(
GEOMETRIC_REPRESENTATION_CONTEXT(3)
GLOBAL_UNCERTAINTY_ASSIGNED_CONTEXT((#19450))
GLOBAL_UNIT_ASSIGNED_CONTEXT((#19472,#19474,#19475))
REPRESENTATION_CONTEXT('','3D')
);
#19464=(
GEOMETRIC_REPRESENTATION_CONTEXT(3)
GLOBAL_UNCERTAINTY_ASSIGNED_CONTEXT((#19451))
GLOBAL_UNIT_ASSIGNED_CONTEXT((#19472,#19474,#19475))
REPRESENTATION_CONTEXT('','3D')
);
#19465=(
GEOMETRIC_REPRESENTATION_CONTEXT(3)
GLOBAL_UNCERTAINTY_ASSIGNED_CONTEXT((#19452))
GLOBAL_UNIT_ASSIGNED_CONTEXT((#19472,#19474,#19475))
REPRESENTATION_CONTEXT('','3D')
);
#19466=(
GEOMETRIC_REPRESENTATION_CONTEXT(3)
GLOBAL_UNCERTAINTY_ASSIGNED_CONTEXT((#19453))
GLOBAL_UNIT_ASSIGNED_CONTEXT((#19472,#19474,#19475))
REPRESENTATION_CONTEXT('','3D')
);
#19467=(
GEOMETRIC_REPRESENTATION_CONTEXT(3)
GLOBAL_UNCERTAINTY_ASSIGNED_CONTEXT((#19454))
GLOBAL_UNIT_ASSIGNED_CONTEXT((#19472,#19474,#19475))
REPRESENTATION_CONTEXT('','3D')
);
#19468=(
GEOMETRIC_REPRESENTATION_CONTEXT(3)
GLOBAL_UNCERTAINTY_ASSIGNED_CONTEXT((#19455))
GLOBAL_UNIT_ASSIGNED_CONTEXT((#19472,#19474,#19475))
REPRESENTATION_CONTEXT('','3D')
);
#19469=(
GEOMETRIC_REPRESENTATION_CONTEXT(3)
GLOBAL_UNCERTAINTY_ASSIGNED_CONTEXT((#19456))
GLOBAL_UNIT_ASSIGNED_CONTEXT((#19472,#19474,#19475))
REPRESENTATION_CONTEXT('','3D')
);
#19470=(
GEOMETRIC_REPRESENTATION_CONTEXT(3)
GLOBAL_UNCERTAINTY_ASSIGNED_CONTEXT((#19457))
GLOBAL_UNIT_ASSIGNED_CONTEXT((#19472,#19474,#19475))
REPRESENTATION_CONTEXT('','3D')
);
#19471=(
GEOMETRIC_REPRESENTATION_CONTEXT(3)
GLOBAL_UNCERTAINTY_ASSIGNED_CONTEXT((#19458))
GLOBAL_UNIT_ASSIGNED_CONTEXT((#19472,#19474,#19475))
REPRESENTATION_CONTEXT('','3D')
);
#19472=(
LENGTH_UNIT()
NAMED_UNIT(*)
SI_UNIT(.CENTI.,.METRE.)
);
#19473=(
LENGTH_UNIT()
NAMED_UNIT(*)
SI_UNIT($,.METRE.)
);
#19474=(
NAMED_UNIT(*)
PLANE_ANGLE_UNIT()
SI_UNIT($,.RADIAN.)
);
#19475=(
NAMED_UNIT(*)
SI_UNIT($,.STERADIAN.)
SOLID_ANGLE_UNIT()
);
#19476=SHAPE_DEFINITION_REPRESENTATION(#19488,#19516);
#19477=SHAPE_DEFINITION_REPRESENTATION(#19489,#19517);
#19478=SHAPE_DEFINITION_REPRESENTATION(#19490,#19518);
#19479=SHAPE_DEFINITION_REPRESENTATION(#19491,#19519);
#19480=SHAPE_DEFINITION_REPRESENTATION(#19492,#19520);
#19481=SHAPE_DEFINITION_REPRESENTATION(#19493,#19521);
#19482=SHAPE_DEFINITION_REPRESENTATION(#19494,#19522);
#19483=SHAPE_DEFINITION_REPRESENTATION(#19495,#19523);
#19484=SHAPE_DEFINITION_REPRESENTATION(#19496,#19524);
#19485=SHAPE_DEFINITION_REPRESENTATION(#19497,#19525);
#19486=SHAPE_DEFINITION_REPRESENTATION(#19498,#19526);
#19487=SHAPE_DEFINITION_REPRESENTATION(#19507,#19527);
#19488=PRODUCT_DEFINITION_SHAPE('',$,#19529);
#19489=PRODUCT_DEFINITION_SHAPE('',$,#19530);
#19490=PRODUCT_DEFINITION_SHAPE('',$,#19531);
#19491=PRODUCT_DEFINITION_SHAPE('',$,#19532);
#19492=PRODUCT_DEFINITION_SHAPE('',$,#19533);
#19493=PRODUCT_DEFINITION_SHAPE('',$,#19534);
#19494=PRODUCT_DEFINITION_SHAPE('',$,#19535);
#19495=PRODUCT_DEFINITION_SHAPE('',$,#19536);
#19496=PRODUCT_DEFINITION_SHAPE('',$,#19537);
#19497=PRODUCT_DEFINITION_SHAPE('',$,#19538);
#19498=PRODUCT_DEFINITION_SHAPE('',$,#19539);
#19499=PRODUCT_DEFINITION_SHAPE($,$,#59);
#19500=PRODUCT_DEFINITION_SHAPE($,$,#60);
#19501=PRODUCT_DEFINITION_SHAPE($,$,#61);
#19502=PRODUCT_DEFINITION_SHAPE($,$,#62);
#19503=PRODUCT_DEFINITION_SHAPE($,$,#63);
#19504=PRODUCT_DEFINITION_SHAPE($,$,#64);
#19505=PRODUCT_DEFINITION_SHAPE($,$,#65);
#19506=PRODUCT_DEFINITION_SHAPE($,$,#66);
#19507=PRODUCT_DEFINITION_SHAPE('',$,#19540);
#19508=PRODUCT_DEFINITION_SHAPE($,$,#67);
#19509=PRODUCT_DEFINITION_SHAPE($,$,#68);
#19510=PRODUCT_DEFINITION_SHAPE($,$,#69);
#19511=PRODUCT_DEFINITION_SHAPE($,$,#70);
#19512=PRODUCT_DEFINITION_SHAPE($,$,#71);
#19513=PRODUCT_DEFINITION_SHAPE($,$,#72);
#19514=PRODUCT_DEFINITION_SHAPE($,$,#73);
#19515=PRODUCT_DEFINITION_SHAPE($,$,#74);
#19516=SHAPE_REPRESENTATION('',(#7272,#7811,#7812,#7813,#7814,#7815,#7816,
#7817,#7818),#19459);
#19517=SHAPE_REPRESENTATION('',(#7273),#19460);
#19518=SHAPE_REPRESENTATION('',(#7333),#19461);
#19519=SHAPE_REPRESENTATION('',(#7393),#19462);
#19520=SHAPE_REPRESENTATION('',(#7411),#19463);
#19521=SHAPE_REPRESENTATION('',(#7422,#7794,#7795,#7796,#7797,#7798,#7799,
#7800,#7801),#19464);
#19522=SHAPE_REPRESENTATION('',(#7423),#19465);
#19523=SHAPE_REPRESENTATION('',(#7525),#19466);
#19524=SHAPE_REPRESENTATION('',(#7633),#19467);
#19525=SHAPE_REPRESENTATION('',(#7686),#19468);
#19526=SHAPE_REPRESENTATION('',(#7768),#19469);
#19527=SHAPE_REPRESENTATION('',(#7802),#19470);
#19528=PRODUCT_DEFINITION_CONTEXT('part definition',#19566,'design');
#19529=PRODUCT_DEFINITION('TOOL-019','TOOL-019',#19541,#19528);
#19530=PRODUCT_DEFINITION('Forged jaw and handle',
'Forged jaw and handle',#19542,#19528);
#19531=PRODUCT_DEFINITION('Moving jaw and handle',
'Moving jaw and handle',#19543,#19528);
#19532=PRODUCT_DEFINITION('Shoulder pivot pin','Shoulder pivot pin',#19544,
#19528);
#19533=PRODUCT_DEFINITION('Pivot retaining ring','Pivot retaining ring',
#19545,#19528);
#19534=PRODUCT_DEFINITION('Grip handle_custom','Grip handle_custom',#19546,
#19528);
#19535=PRODUCT_DEFINITION('2026-11-10-01-30-02-385',
'Upper structural shell',#19547,#19528);
#19536=PRODUCT_DEFINITION('2026-11-10-01-30-02-390',
'Lower structural shell',#19548,#19528);
#19537=PRODUCT_DEFINITION('2026-11-10-01-30-02-394','Soft grip layer',#19549,
#19528);
#19538=PRODUCT_DEFINITION('2026-11-10-01-30-02-397',
'Socket head cap screw M3x16',#19550,#19528);
#19539=PRODUCT_DEFINITION('2026-11-10-01-30-02-398','Hex nut M3',#19551,
#19528);
#19540=PRODUCT_DEFINITION('Pivot thrust washer','Pivot thrust washer',#19552,
#19528);
#19541=PRODUCT_DEFINITION_FORMATION('',$,#19568);
#19542=PRODUCT_DEFINITION_FORMATION('',$,#19569);
#19543=PRODUCT_DEFINITION_FORMATION('',$,#19570);
#19544=PRODUCT_DEFINITION_FORMATION('',$,#19571);
#19545=PRODUCT_DEFINITION_FORMATION('',$,#19572);
#19546=PRODUCT_DEFINITION_FORMATION('',$,#19573);
#19547=PRODUCT_DEFINITION_FORMATION('',$,#19574);
#19548=PRODUCT_DEFINITION_FORMATION('',$,#19575);
#19549=PRODUCT_DEFINITION_FORMATION('',$,#19576);
#19550=PRODUCT_DEFINITION_FORMATION('',$,#19577);
#19551=PRODUCT_DEFINITION_FORMATION('',$,#19578);
#19552=PRODUCT_DEFINITION_FORMATION('',$,#19579);
#19553=PRODUCT_RELATED_PRODUCT_CATEGORY('TOOL-019','TOOL-019',(#19568));
#19554=PRODUCT_RELATED_PRODUCT_CATEGORY('Forged jaw and handle',
'Forged jaw and handle',(#19569));
#19555=PRODUCT_RELATED_PRODUCT_CATEGORY('Moving jaw and handle',
'Moving jaw and handle',(#19570));
#19556=PRODUCT_RELATED_PRODUCT_CATEGORY('Shoulder pivot pin',
'Shoulder pivot pin',(#19571));
#19557=PRODUCT_RELATED_PRODUCT_CATEGORY('Pivot retaining ring',
'Pivot retaining ring',(#19572));
#19558=PRODUCT_RELATED_PRODUCT_CATEGORY('Grip handle_custom',
'Grip handle_custom',(#19573));
#19559=PRODUCT_RELATED_PRODUCT_CATEGORY('Upper structural shell',
'Upper structural shell',(#19574));
#19560=PRODUCT_RELATED_PRODUCT_CATEGORY('Lower structural shell',
'Lower structural shell',(#19575));
#19561=PRODUCT_RELATED_PRODUCT_CATEGORY('Soft grip layer',
'Soft grip layer',(#19576));
#19562=PRODUCT_RELATED_PRODUCT_CATEGORY('Socket head cap screw M3x16',
'Socket head cap screw M3x16',(#19577));
#19563=PRODUCT_RELATED_PRODUCT_CATEGORY('Hex nut M3','Hex nut M3',(#19578));
#19564=PRODUCT_RELATED_PRODUCT_CATEGORY('Pivot thrust washer',
'Pivot thrust washer',(#19579));
#19565=APPLICATION_PROTOCOL_DEFINITION('international standard',
'automotive_design',2009,#19566);
#19566=APPLICATION_CONTEXT(
'Core Data for Automotive Mechanical Design Process');
#19567=PRODUCT_CONTEXT('part definition',#19566,'mechanical');
#19568=PRODUCT('TOOL-019','TOOL-019',$,(#19567));
#19569=PRODUCT('Forged jaw and handle','Forged jaw and handle',$,(#19567));
#19570=PRODUCT('Moving jaw and handle','Moving jaw and handle',$,(#19567));
#19571=PRODUCT('Shoulder pivot pin','Shoulder pivot pin',$,(#19567));
#19572=PRODUCT('Pivot retaining ring','Pivot retaining ring',$,(#19567));
#19573=PRODUCT('Grip handle_custom','Grip handle_custom',$,(#19567));
#19574=PRODUCT('2026-11-10-01-30-02-385','Upper structural shell',$,(#19567));
#19575=PRODUCT('2026-11-10-01-30-02-390','Lower structural shell',$,(#19567));
#19576=PRODUCT('2026-11-10-01-30-02-394','Soft grip layer',$,(#19567));
#19577=PRODUCT('2026-11-10-01-30-02-397','Socket head cap screw M3x16',
$,(#19567));
#19578=PRODUCT('2026-11-10-01-30-02-398','Hex nut M3',$,(#19567));
#19579=PRODUCT('Pivot thrust washer','Pivot thrust washer',$,(#19567));
#19580=PRESENTATION_STYLE_ASSIGNMENT((#19588));
#19581=PRESENTATION_STYLE_ASSIGNMENT((#19589));
#19582=PRESENTATION_STYLE_ASSIGNMENT((#19590));
#19583=PRESENTATION_STYLE_ASSIGNMENT((#19591));
#19584=PRESENTATION_STYLE_ASSIGNMENT((#19592));
#19585=PRESENTATION_STYLE_ASSIGNMENT((#19593));
#19586=PRESENTATION_STYLE_ASSIGNMENT((#19594));
#19587=PRESENTATION_STYLE_ASSIGNMENT((#19595));
#19588=SURFACE_STYLE_USAGE(.BOTH.,#19596);
#19589=SURFACE_STYLE_USAGE(.BOTH.,#19597);
#19590=SURFACE_STYLE_USAGE(.BOTH.,#19598);
#19591=SURFACE_STYLE_USAGE(.BOTH.,#19599);
#19592=SURFACE_STYLE_USAGE(.BOTH.,#19600);
#19593=SURFACE_STYLE_USAGE(.BOTH.,#19601);
#19594=SURFACE_STYLE_USAGE(.BOTH.,#19602);
#19595=SURFACE_STYLE_USAGE(.BOTH.,#19603);
#19596=SURFACE_SIDE_STYLE('',(#19604));
#19597=SURFACE_SIDE_STYLE('',(#19605));
#19598=SURFACE_SIDE_STYLE('',(#19606));
#19599=SURFACE_SIDE_STYLE('',(#19607));
#19600=SURFACE_SIDE_STYLE('',(#19608));
#19601=SURFACE_SIDE_STYLE('',(#19609));
#19602=SURFACE_SIDE_STYLE('',(#19610));
#19603=SURFACE_SIDE_STYLE('',(#19611));
#19604=SURFACE_STYLE_FILL_AREA(#19612);
#19605=SURFACE_STYLE_FILL_AREA(#19613);
#19606=SURFACE_STYLE_FILL_AREA(#19614);
#19607=SURFACE_STYLE_FILL_AREA(#19615);
#19608=SURFACE_STYLE_FILL_AREA(#19616);
#19609=SURFACE_STYLE_FILL_AREA(#19617);
#19610=SURFACE_STYLE_FILL_AREA(#19618);
#19611=SURFACE_STYLE_FILL_AREA(#19619);
#19612=FILL_AREA_STYLE('Steel - Satin',(#19620));
#19613=FILL_AREA_STYLE('Tool steel gray',(#19621));
#19614=FILL_AREA_STYLE('Pivot dark gray',(#19622));
#19615=FILL_AREA_STYLE('Dark gray',(#19623));
#19616=FILL_AREA_STYLE('Structural dark blue',(#19624));
#19617=FILL_AREA_STYLE('Sky blue soft grip',(#19625));
#19618=FILL_AREA_STYLE('Fastener gray',(#19626));
#19619=FILL_AREA_STYLE('Washer gray',(#19627));
#19620=FILL_AREA_STYLE_COLOUR('Steel - Satin',#19628);
#19621=FILL_AREA_STYLE_COLOUR('Tool steel gray',#19629);
#19622=FILL_AREA_STYLE_COLOUR('Pivot dark gray',#19630);
#19623=FILL_AREA_STYLE_COLOUR('Dark gray',#19631);
#19624=FILL_AREA_STYLE_COLOUR('Structural dark blue',#19632);
#19625=FILL_AREA_STYLE_COLOUR('Sky blue soft grip',#19633);
#19626=FILL_AREA_STYLE_COLOUR('Fastener gray',#19634);
#19627=FILL_AREA_STYLE_COLOUR('Washer gray',#19635);
#19628=COLOUR_RGB('Steel - Satin',0.627450980392157,0.627450980392157,0.627450980392157);
#19629=COLOUR_RGB('Tool steel gray',0.607843137254902,0.643137254901961,
0.698039215686274);
#19630=COLOUR_RGB('Pivot dark gray',0.27843137254902,0.309803921568627,
0.352941176470588);
#19631=COLOUR_RGB('Dark gray',0.250980392156863,0.282352941176471,0.32156862745098);
#19632=COLOUR_RGB('Structural dark blue',0.0901960784313725,0.270588235294118,
0.513725490196078);
#19633=COLOUR_RGB('Sky blue soft grip',0.662745098039216,0.831372549019608,
0.949019607843137);
#19634=COLOUR_RGB('Fastener gray',0.607843137254902,0.643137254901961,0.698039215686274);
#19635=COLOUR_RGB('Washer gray',0.725490196078431,0.752941176470588,0.792156862745098);
ENDSEC;
END-ISO-10303-21;
